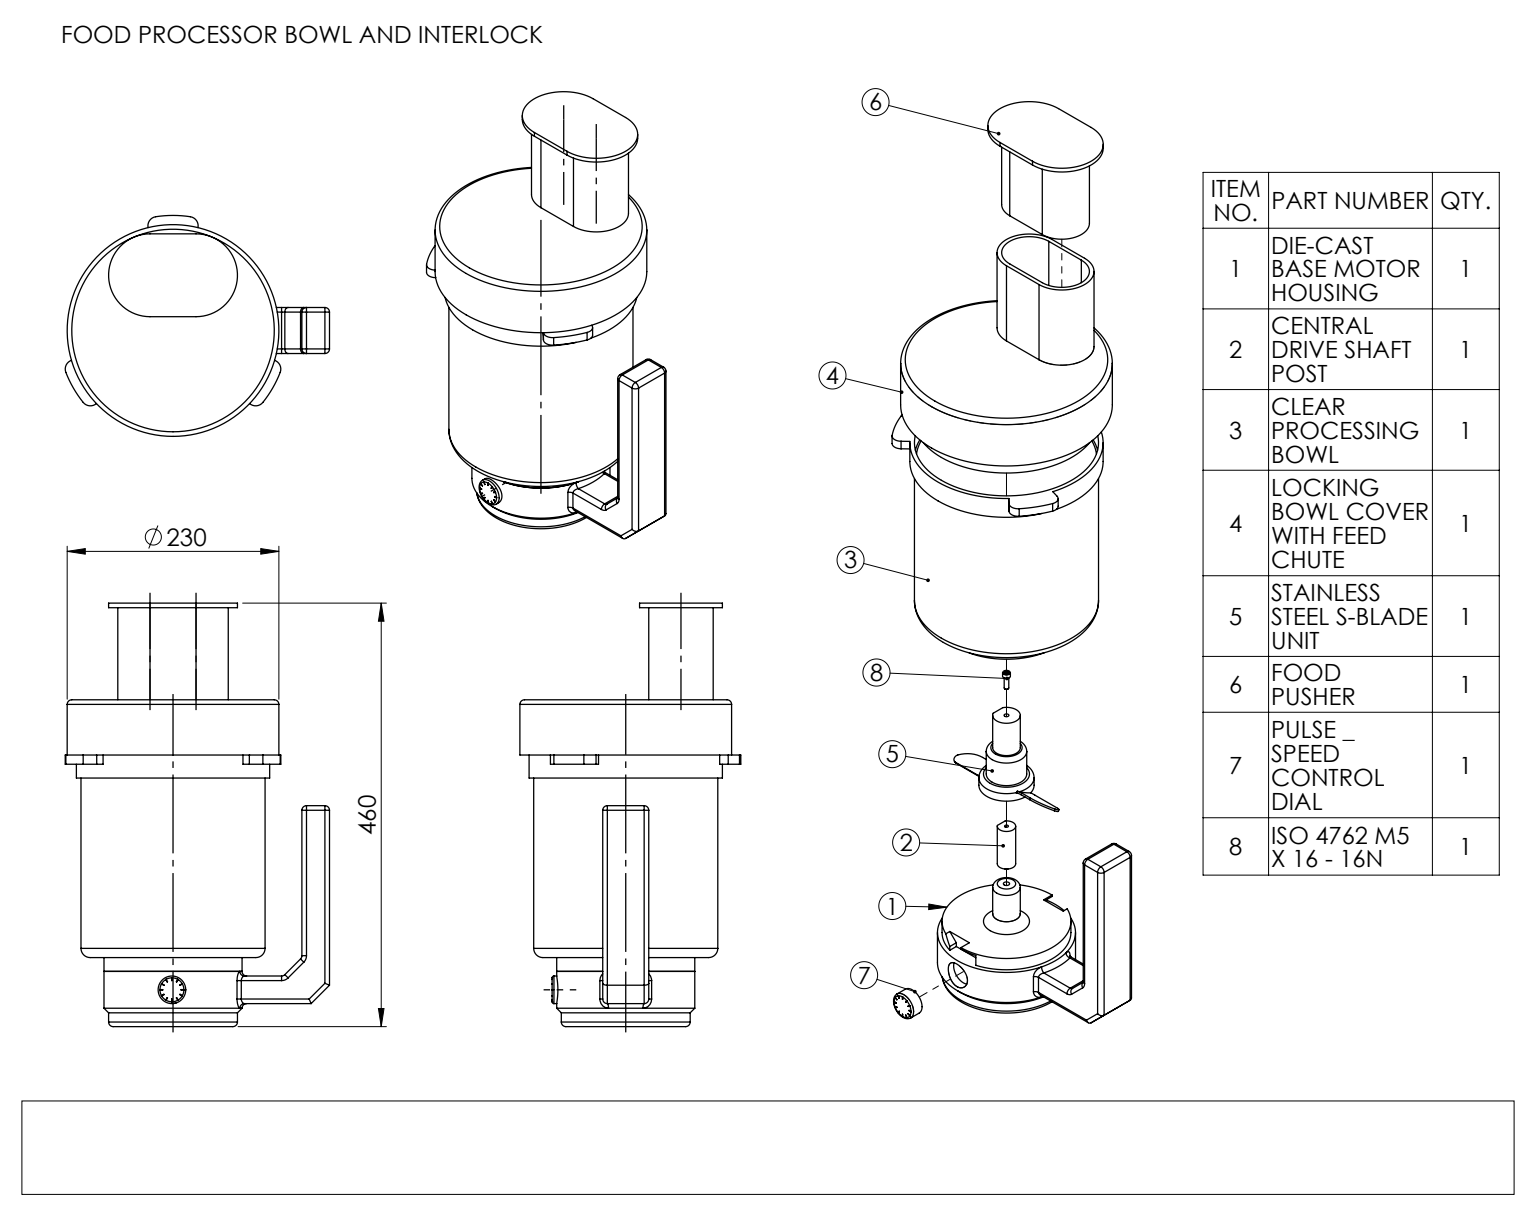
ISO-10303-21;
HEADER;
FILE_DESCRIPTION (('STEP AP214'),
    '1' );
FILE_NAME ('BR-821',
    '2026-10-08T14:59:03',
    ( '' ),
    ( '' ),
    'SwSTEP 2.0',
    'SolidWorks 2026',
    '' );
FILE_SCHEMA (( 'AUTOMOTIVE_DESIGN' ));
ENDSEC;

DATA;
#1 = ORIENTED_EDGE ( 'NONE', *, *, #9406, .F. ) ;
#2 = CARTESIAN_POINT ( 'NONE',  ( 11.80921887069467324, 30.25000000000018474, 79.50000000000000000 ) ) ;
#3 = CARTESIAN_POINT ( 'NONE',  ( 71.93323519045090109, 49.64954395535312415, 21.22984507177767100 ) ) ;
#4 = ORIENTED_EDGE ( 'NONE', *, *, #10707, .F. ) ;
#5 = LINE ( 'NONE', #4817, #10432 ) ;
#6 = PLANE ( 'NONE',  #104 ) ;
#7 = AXIS2_PLACEMENT_3D ( 'NONE', #9543, #8426, #7563 ) ;
#8 = VERTEX_POINT ( 'NONE', #10428 ) ;
#9 = MECHANICAL_DESIGN_GEOMETRIC_PRESENTATION_REPRESENTATION (  '', ( #5399 ), #3796 ) ;
#10 = CARTESIAN_POINT ( 'NONE',  ( 1.836970198721029589E-15, 110.0000000000000000, 15.00000000000000000 ) ) ;
#11 = LINE ( 'NONE', #6448, #10967 ) ;
#12 = CARTESIAN_POINT ( 'NONE',  ( -25.00000000000000000, 445.0000000000000568, -90.00000000000000000 ) ) ;
#13 = CARTESIAN_POINT ( 'NONE',  ( -2.298097038856279806, 112.6250000000000000, -2.298097038856279362 ) ) ;
#14 = CARTESIAN_POINT ( 'NONE',  ( 1.658621287961228320E-16, 111.8124999986344079, 2.708734124999999882 ) ) ;
#15 = ORIENTED_EDGE ( 'NONE', *, *, #10225, .T. ) ;
#16 = AXIS2_PLACEMENT_3D ( 'NONE', #8718, #1999, #3870 ) ;
#17 = ORIENTED_EDGE ( 'NONE', *, *, #3705, .T. ) ;
#18 = CYLINDRICAL_SURFACE ( 'NONE', #1272, 5.000000000000001776 ) ;
#19 = EDGE_CURVE ( 'NONE', #6749, #65, #10302, .T. ) ;
#20 = DIRECTION ( 'NONE',  ( 0.4999999999999933387, -0.8660254037844424824, 0.000000000000000000 ) ) ;
#21 = ORIENTED_EDGE ( 'NONE', *, *, #5442, .F. ) ;
#22 = VECTOR ( 'NONE', #10909, 1000.000000000000000 ) ;
#23 = CARTESIAN_POINT ( 'NONE',  ( -7.907287480251413925, 18.86666975080236597, 80.00000000000000000 ) ) ;
#24 = DIRECTION ( 'NONE',  ( 0.000000000000000000, 0.000000000000000000, -1.000000000000000000 ) ) ;
#25 = CARTESIAN_POINT ( 'NONE',  ( -30.63265341208206038, 76.40790137508867019, 5.685798939282528330 ) ) ;
#26 = CARTESIAN_POINT ( 'NONE',  ( 0.000000000000000000, 153.0000000000000000, 2.099999999999998312 ) ) ;
#27 = EDGE_CURVE ( 'NONE', #1251, #10198, #9485, .T. ) ;
#28 = ORIENTED_EDGE ( 'NONE', *, *, #12033, .F. ) ;
#29 = FACE_OUTER_BOUND ( 'NONE', #6935, .T. ) ;
#30 = UNCERTAINTY_MEASURE_WITH_UNIT (LENGTH_MEASURE( 1.000000000000000082E-05 ), #8409, 'distance_accuracy_value', 'NONE');
#31 = CARTESIAN_POINT ( 'NONE',  ( 74.19588822391826000, 40.66783446091307042, -24.95803700703555350 ) ) ;
#32 = SURFACE_STYLE_FILL_AREA ( #12272 ) ;
#33 = CARTESIAN_POINT ( 'NONE',  ( 0.000000000000000000, 62.00000000000000000, 0.000000000000000000 ) ) ;
#34 = DIRECTION ( 'NONE',  ( 0.000000000000000000, -0.000000000000000000, 1.000000000000000000 ) ) ;
#35 = CARTESIAN_POINT ( 'NONE',  ( 3.250000000000000444, 113.0625000000000000, 1.346194077712559167 ) ) ;
#36 = CARTESIAN_POINT ( 'NONE',  ( 77.29209776116614705, 15.00000000000009059, -20.32449628861697377 ) ) ;
#37 = ORIENTED_EDGE ( 'NONE', *, *, #7691, .T. ) ;
#38 = FACE_BOUND ( 'NONE', #4194, .T. ) ;
#39 = EDGE_CURVE ( 'NONE', #10896, #4898, #9360, .T. ) ;
#40 = CARTESIAN_POINT ( 'NONE',  ( -1.440781129305471087, 43.00000000000008527, 80.00000000000000000 ) ) ;
#41 = VECTOR ( 'NONE', #11324, 1000.000000000000000 ) ;
#42 = ORIENTED_EDGE ( 'NONE', *, *, #4224, .F. ) ;
#43 = CYLINDRICAL_SURFACE ( 'NONE', #5992, 70.00000000000001421 ) ;
#44 = VERTEX_POINT ( 'NONE', #11902 ) ;
#45 = VECTOR ( 'NONE', #2118, 1000.000000000000000 ) ;
#46 = LINE ( 'NONE', #5798, #12120 ) ;
#47 = LINE ( 'NONE', #9767, #6437 ) ;
#48 = EDGE_LOOP ( 'NONE', ( #1031, #6053, #2883, #3031 ) ) ;
#49 = CARTESIAN_POINT ( 'NONE',  ( 30.43737458073258040, 77.00000000000001421, -5.702507482421638407 ) ) ;
#50 = CARTESIAN_POINT ( 'NONE',  ( 170.0000000000011369, 35.00000000000004974, -19.99999999999999645 ) ) ;
#51 = VERTEX_POINT ( 'NONE', #2763 ) ;
#52 = ADVANCED_FACE ( 'NONE', ( #8078 ), #12195, .T. ) ;
#53 = PLANE ( 'NONE',  #708 ) ;
#54 = DIRECTION ( 'NONE',  ( -0.000000000000000000, -1.000000000000000000, -0.000000000000000000 ) ) ;
#55 = DIRECTION ( 'NONE',  ( -0.000000000000000000, -1.000000000000000000, -0.000000000000000000 ) ) ;
#56 = ORIENTED_EDGE ( 'NONE', *, *, #12103, .T. ) ;
#57 = CARTESIAN_POINT ( 'NONE',  ( -1.915364268218909150, 112.6874999986344079, 1.915364268218909594 ) ) ;
#58 = VECTOR ( 'NONE', #5099, 1000.000000000000000 ) ;
#59 = DIRECTION ( 'NONE',  ( 0.000000000000000000, -0.4999999999999976685, 0.8660254037844399289 ) ) ;
#60 = ORIENTED_EDGE ( 'NONE', *, *, #4267, .T. ) ;
#61 = ADVANCED_FACE ( 'NONE', ( #9422 ), #904, .T. ) ;
#62 = CARTESIAN_POINT ( 'NONE',  ( -25.00000000000000000, 345.0000000000000568, -90.00000000000000000 ) ) ;
#63 = ADVANCED_FACE ( 'NONE', ( #7151 ), #4694, .T. ) ;
#64 = CARTESIAN_POINT ( 'NONE',  ( -5.632982942078911925, 15.66369320862007264, 74.78974241430267966 ) ) ;
#65 = VERTEX_POINT ( 'NONE', #3417 ) ;
#66 = CARTESIAN_POINT ( 'NONE',  ( 2.500000000000000000, -1.178949249685214307, 2.042000000000001592 ) ) ;
#67 = ORIENTED_EDGE ( 'NONE', *, *, #12135, .T. ) ;
#68 = AXIS2_PLACEMENT_3D ( 'NONE', #1472, #532, #4327 ) ;
#69 = AXIS2_PLACEMENT_3D ( 'NONE', #2443, #8100, #4365 ) ;
#70 = CARTESIAN_POINT ( 'NONE',  ( -25.00000000000000000, 347.0000000000000568, -88.00000000000000000 ) ) ;
#71 = CARTESIAN_POINT ( 'NONE',  ( 100.7495955565343593, 285.0000000000000568, 29.57226733266770680 ) ) ;
#72 = FACE_BOUND ( 'NONE', #11694, .T. ) ;
#73 = CARTESIAN_POINT ( 'NONE',  ( 5.525725221640833240, 18.86666975080242992, 79.50000000000000000 ) ) ;
#74 = CARTESIAN_POINT ( 'NONE',  ( -3.250000000000000444, 111.5000000000000000, 3.980102097228898231E-16 ) ) ;
#75 = CARTESIAN_POINT ( 'NONE',  ( 72.29554967163173274, 10.06394264408140771, 19.96827991394381030 ) ) ;
#76 = ORIENTED_EDGE ( 'NONE', *, *, #6927, .T. ) ;
#77 = PRESENTATION_STYLE_ASSIGNMENT (( #1089 ) ) ;
#78 = AXIS2_PLACEMENT_3D ( 'NONE', #1523, #2574, #3573 ) ;
#79 = AXIS2_PLACEMENT_3D ( 'NONE', #1491, #4293, #8024 ) ;
#80 = VERTEX_POINT ( 'NONE', #3761 ) ;
#81 = CYLINDRICAL_SURFACE ( 'NONE', #3664, 5.000000000000000888 ) ;
#82 = CYLINDRICAL_SURFACE ( 'NONE', #2511, 15.00000000000000000 ) ;
#83 = EDGE_LOOP ( 'NONE', ( #1644, #11783, #306, #9102 ) ) ;
#84 = DIRECTION ( 'NONE',  ( 0.000000000000000000, 0.000000000000000000, 1.000000000000000000 ) ) ;
#85 = DIRECTION ( 'NONE',  ( -0.000000000000000000, -1.000000000000000000, -0.000000000000000000 ) ) ;
#86 = DIRECTION ( 'NONE',  ( 0.000000000000000000, 1.000000000000000000, 0.000000000000000000 ) ) ;
#87 = CIRCLE ( 'NONE', #695, 73.00000000000002842 ) ;
#88 = AXIS2_PLACEMENT_3D ( 'NONE', #4376, #577, #4254 ) ;
#89 = EDGE_CURVE ( 'NONE', #9269, #3272, #10464, .T. ) ;
#90 = ORIENTED_EDGE ( 'NONE', *, *, #4166, .T. ) ;
#91 = EDGE_CURVE ( 'NONE', #9396, #343, #11975, .T. ) ;
#92 = ADVANCED_FACE ( 'NONE', ( #6517 ), #10949, .F. ) ;
#93 = VECTOR ( 'NONE', #163, 1000.000000000000000 ) ;
#94 = CARTESIAN_POINT ( 'NONE',  ( 74.77359728361332714, 42.68513822356444365, -24.22100760279283094 ) ) ;
#95 = AXIS2_PLACEMENT_3D ( 'NONE', #7431, #12111, #3682 ) ;
#96 = CARTESIAN_POINT ( 'NONE',  ( -1.440781129305282571, 17.00000000000009592, 80.00000000000000000 ) ) ;
#97 = CARTESIAN_POINT ( 'NONE',  ( 25.00000000000000000, 445.0000000000000568, -59.99999999999999289 ) ) ;
#98 = DIRECTION ( 'NONE',  ( 1.000000000000000000, 0.000000000000000000, -3.469446951953613203E-16 ) ) ;
#99 = FACE_OUTER_BOUND ( 'NONE', #3781, .T. ) ;
#100 = ORIENTED_EDGE ( 'NONE', *, *, #2094, .T. ) ;
#101 = CARTESIAN_POINT ( 'NONE',  ( -2.298097038856279362, 111.3750000000000000, 2.298097038856279806 ) ) ;
#102 = PRODUCT ( 'Food Pusher', 'Food Pusher', '', ( #178 ) ) ;
#103 = CARTESIAN_POINT ( 'NONE',  ( 1.121994411437818862, 110.4999999986344079, 2.708734125000000326 ) ) ;
#104 = AXIS2_PLACEMENT_3D ( 'NONE', #11679, #5881, #9664 ) ;
#105 = ORIENTED_EDGE ( 'NONE', *, *, #968, .F. ) ;
#106 = DIRECTION ( 'NONE',  ( -0.000000000000000000, -1.000000000000000000, -0.000000000000000000 ) ) ;
#107 = AXIS2_PLACEMENT_3D ( 'NONE', #11604, #10713, #5802 ) ;
#108 = VERTEX_POINT ( 'NONE', #8368 ) ;
#109 = CARTESIAN_POINT ( 'NONE',  ( 0.000000000000000000, 67.00000000000000000, -73.00000000000002842 ) ) ;
#110 = DIRECTION ( 'NONE',  ( -0.8660254037844363761, 0.5000000000000038858, 0.000000000000000000 ) ) ;
#111 = ORIENTED_EDGE ( 'NONE', *, *, #6676, .F. ) ;
#112 = AXIS2_PLACEMENT_3D ( 'NONE', #12229, #2739, #12169 ) ;
#113 = DIRECTION ( 'NONE',  ( 0.000000000000000000, 1.000000000000000000, 0.000000000000000000 ) ) ;
#114 = CARTESIAN_POINT ( 'NONE',  ( 27.33018067101281900, 86.99999999999998579, 12.37179148263487782 ) ) ;
#115 = ORIENTED_EDGE ( 'NONE', *, *, #11098, .T. ) ;
#116 = CONTEXT_DEPENDENT_SHAPE_REPRESENTATION ( #11241, #9863 ) ;
#117 = DIRECTION ( 'NONE',  ( 1.000000000000000000, -0.000000000000000000, 0.000000000000000000 ) ) ;
#118 = COLOUR_RGB ( '', 0.09019608, 0.27058824, 0.51372549) ;
#119 = LINE ( 'NONE', #1007, #8979 ) ;
#120 = DIRECTION ( 'NONE',  ( -0.2816406412635021894, 0.000000000000000000, 0.9595199576812789566 ) ) ;
#121 = ORIENTED_EDGE ( 'NONE', *, *, #6558, .F. ) ;
#122 = CARTESIAN_POINT ( 'NONE',  ( -1.121994411437818862, 113.6249999986344079, 2.708734125000000326 ) ) ;
#123 = DIRECTION ( 'NONE',  ( 1.000000000000000000, 0.000000000000000000, 0.000000000000000000 ) ) ;
#124 = EDGE_CURVE ( 'NONE', #2418, #8492, #10933, .T. ) ;
#125 = AXIS2_PLACEMENT_3D ( 'NONE', #9417, #9481, #11434 ) ;
#126 = EDGE_LOOP ( 'NONE', ( #8083, #10579, #5308 ) ) ;
#127 = CARTESIAN_POINT ( 'NONE',  ( 89.80805993797383735, 285.0000000000000568, 71.82974571984303225 ) ) ;
#128 = PLANE ( 'NONE',  #8446 ) ;
#129 = ORIENTED_EDGE ( 'NONE', *, *, #8171, .F. ) ;
#130 = CARTESIAN_POINT ( 'NONE',  ( 1.836970198721029589E-15, 115.0000000000000142, 15.00000000000000000 ) ) ;
#131 = DIRECTION ( 'NONE',  ( -1.000000000000000000, -1.387778780781444492E-15, 0.000000000000000000 ) ) ;
#132 = ORIENTED_EDGE ( 'NONE', *, *, #1282, .T. ) ;
#133 = CARTESIAN_POINT ( 'NONE',  ( -1.346194077712560944, 110.3125000000000000, 3.249999999999998668 ) ) ;
#134 = CARTESIAN_POINT ( 'NONE',  ( 69.52686081652184669, 20.00000000000009237, -28.12499999999999645 ) ) ;
#135 = PLANE ( 'NONE',  #4004 ) ;
#136 = CARTESIAN_POINT ( 'NONE',  ( 1.915364268218908705, 114.4374999986344079, -1.915364268218909594 ) ) ;
#137 = CARTESIAN_POINT ( 'NONE',  ( 20.00000000000000000, 7.965803112215716020, -67.08203932499371547 ) ) ;
#138 = CARTESIAN_POINT ( 'NONE',  ( 1.915364268218909150, 112.6874999986344079, 1.915364268218909150 ) ) ;
#139 = ORIENTED_EDGE ( 'NONE', *, *, #323, .F. ) ;
#140 = EDGE_CURVE ( 'NONE', #6671, #381, #10679, .T. ) ;
#141 = ADVANCED_FACE ( 'NONE', ( #5767 ), #10055, .F. ) ;
#142 = EDGE_LOOP ( 'NONE', ( #5615, #3837, #7263, #6163, #8146, #5499, #6846 ) ) ;
#143 = PLANE ( 'NONE',  #4255 ) ;
#144 = DIRECTION ( 'NONE',  ( -0.000000000000000000, -1.000000000000000000, -0.000000000000000000 ) ) ;
#145 = ORIENTED_EDGE ( 'NONE', *, *, #5135, .F. ) ;
#146 = CARTESIAN_POINT ( 'NONE',  ( -75.98513253586241945, 285.0000000000000568, 72.46557550663233371 ) ) ;
#147 = CARTESIAN_POINT ( 'NONE',  ( 75.98513253586142469, 275.0000000000000000, 72.46557550663338532 ) ) ;
#148 = ADVANCED_FACE ( 'NONE', ( #9407 ), #4682, .T. ) ;
#149 = DIRECTION ( 'NONE',  ( -0.000000000000000000, -0.000000000000000000, 1.000000000000000000 ) ) ;
#150 = CARTESIAN_POINT ( 'NONE',  ( -0.9407811293052614765, 20.00000000000009237, 79.50000000000000000 ) ) ;
#151 = ORIENTED_EDGE ( 'NONE', *, *, #4389, .T. ) ;
#152 = AXIS2_PLACEMENT_3D ( 'NONE', #2615, #6425, #9273 ) ;
#153 = EDGE_CURVE ( 'NONE', #12150, #6802, #1695, .T. ) ;
#154 = EDGE_CURVE ( 'NONE', #8296, #4939, #9365, .T. ) ;
#155 = FILL_AREA_STYLE_COLOUR ( '', #11172 ) ;
#156 = ORIENTED_EDGE ( 'NONE', *, *, #11948, .T. ) ;
#157 = CARTESIAN_POINT ( 'NONE',  ( 70.81305327821827689, 40.84876555524851938, -24.93520811514266100 ) ) ;
#158 = AXIS2_PLACEMENT_3D ( 'NONE', #4049, #10649, #3342 ) ;
#159 = CARTESIAN_POINT ( 'NONE',  ( 9.942549119892305498, 36.71650635094628967, 79.50000000000000000 ) ) ;
#160 = MECHANICAL_DESIGN_GEOMETRIC_PRESENTATION_REPRESENTATION (  '', ( #10913 ), #2162 ) ;
#161 = CARTESIAN_POINT ( 'NONE',  ( 0.000000000000000000, 264.9990000000000236, -34.99999999999999289 ) ) ;
#162 = ORIENTED_EDGE ( 'NONE', *, *, #3844, .F. ) ;
#163 = DIRECTION ( 'NONE',  ( -0.000000000000000000, -1.000000000000000000, -0.000000000000000000 ) ) ;
#164 = CARTESIAN_POINT ( 'NONE',  ( 76.56941542346943663, 15.25646994755911656, -21.58911091692574047 ) ) ;
#165 = ORIENTED_EDGE ( 'NONE', *, *, #7969, .F. ) ;
#166 = CARTESIAN_POINT ( 'NONE',  ( 1.224646799147353533E-14, 265.0000000000000000, -100.0000000000000284 ) ) ;
#167 = CARTESIAN_POINT ( 'NONE',  ( 1.658621287961228566E-16, 110.5624999986344079, 2.708734125000000326 ) ) ;
#168 = ORIENTED_EDGE ( 'NONE', *, *, #9268, .F. ) ;
#169 = CARTESIAN_POINT ( 'NONE',  ( -9.976035167149731819, 34.78349364905394481, 80.00000000000000000 ) ) ;
#170 = ORIENTED_EDGE ( 'NONE', *, *, #8169, .T. ) ;
#171 = LINE ( 'NONE', #7782, #5342 ) ;
#172 = DIRECTION ( 'NONE',  ( 1.000000000000000000, 0.000000000000000000, 3.469446951953613203E-16 ) ) ;
#173 = EDGE_LOOP ( 'NONE', ( #129, #2028 ) ) ;
#174 = CARTESIAN_POINT ( 'NONE',  ( 30.14540500433760783, 76.99999999999997158, -4.927060346216586950 ) ) ;
#175 = EDGE_CURVE ( 'NONE', #10718, #2926, #1576, .T. ) ;
#176 = FACE_OUTER_BOUND ( 'NONE', #3457, .T. ) ;
#177 = ORIENTED_EDGE ( 'NONE', *, *, #6032, .T. ) ;
#178 = PRODUCT_CONTEXT ( 'NONE', #12278, 'mechanical' ) ;
#179 = VECTOR ( 'NONE', #1966, 1000.000000000000000 ) ;
#180 = CARTESIAN_POINT ( 'NONE',  ( 11.80921887069467324, 30.00000000000008882, 80.00000000000000000 ) ) ;
#181 = DIRECTION ( 'NONE',  ( 0.000000000000000000, -0.000000000000000000, 1.000000000000000000 ) ) ;
#182 = ORIENTED_EDGE ( 'NONE', *, *, #8491, .F. ) ;
#183 = CARTESIAN_POINT ( 'NONE',  ( -2.708734125000000326, 113.7499999986343937, 1.121994411437818862 ) ) ;
#184 = CARTESIAN_POINT ( 'NONE',  ( -5.970153145843347347E-16, 113.6249999972688158, -3.250000000000000444 ) ) ;
#185 = AXIS2_PLACEMENT_3D ( 'NONE', #6233, #8025, #4294 ) ;
#186 = ORIENTED_EDGE ( 'NONE', *, *, #175, .F. ) ;
#187 = DIRECTION ( 'NONE',  ( -1.000000000000000000, 0.000000000000000000, -0.000000000000000000 ) ) ;
#188 = LINE ( 'NONE', #3126, #12048 ) ;
#189 = ORIENTED_EDGE ( 'NONE', *, *, #4744, .F. ) ;
#190 = DIRECTION ( 'NONE',  ( 0.000000000000000000, 1.000000000000000000, 0.000000000000000000 ) ) ;
#191 = DIRECTION ( 'NONE',  ( -0.5000000000000095479, -0.8660254037844331565, 0.000000000000000000 ) ) ;
#192 = ORIENTED_EDGE ( 'NONE', *, *, #11363, .T. ) ;
#193 = LINE ( 'NONE', #8731, #4891 ) ;
#194 = CARTESIAN_POINT ( 'NONE',  ( 150.0000000000010800, 15.00000000000008882, 20.00000000000000000 ) ) ;
#195 = DIRECTION ( 'NONE',  ( -0.000000000000000000, -0.000000000000000000, 1.000000000000000000 ) ) ;
#196 = EDGE_CURVE ( 'NONE', #8201, #12241, #11240, .T. ) ;
#197 = VECTOR ( 'NONE', #4605, 1000.000000000000000 ) ;
#198 = DIRECTION ( 'NONE',  ( -0.000000000000000000, -1.000000000000000000, 0.000000000000000000 ) ) ;
#199 = CARTESIAN_POINT ( 'NONE',  ( 5.000000000000000888, 0.000000000000000000, 0.000000000000000000 ) ) ;
#200 = EDGE_CURVE ( 'NONE', #12119, #9588, #3746, .T. ) ;
#201 = CARTESIAN_POINT ( 'NONE',  ( 72.61843774138908714, 15.00000000000009059, 18.75000000000000355 ) ) ;
#202 = CIRCLE ( 'NONE', #8371, 5.000000000000000888 ) ;
#203 = ORIENTED_EDGE ( 'NONE', *, *, #11363, .F. ) ;
#204 = VECTOR ( 'NONE', #4922, 1000.000000000000227 ) ;
#205 = ORIENTED_EDGE ( 'NONE', *, *, #4032, .F. ) ;
#206 = VECTOR ( 'NONE', #5383, 1000.000000000000000 ) ;
#207 = PRODUCT ( 'Stainless Steel S-Blade Unit', 'Stainless Steel S-Blade Unit', '', ( #412 ) ) ;
#208 = CARTESIAN_POINT ( 'NONE',  ( 13.11499952929491641, 34.60506461548092716, 73.84520852716261174 ) ) ;
#209 = EDGE_LOOP ( 'NONE', ( #9146, #6174, #8156, #10356 ) ) ;
#210 = DIRECTION ( 'NONE',  ( -0.7071067811865503483, -0.7071067811865447972, -0.000000000000000000 ) ) ;
#211 = DIRECTION ( 'NONE',  ( 0.000000000000000000, 1.000000000000000000, 0.000000000000000000 ) ) ;
#212 = CARTESIAN_POINT ( 'NONE',  ( 0.000000000000000000, 10.00000000000017586, 0.000000000000000000 ) ) ;
#213 = CARTESIAN_POINT ( 'NONE',  ( -7.473072744137204459, 18.61875173514729198, 80.00000000000000000 ) ) ;
#214 = EDGE_CURVE ( 'NONE', #4965, #8588, #3628, .T. ) ;
#215 = EDGE_CURVE ( 'NONE', #8652, #10794, #4622, .T. ) ;
#216 = AXIS2_PLACEMENT_3D ( 'NONE', #7014, #9871, #9743 ) ;
#217 = AXIS2_PLACEMENT_3D ( 'NONE', #5378, #8352, #3567 ) ;
#218 =( LENGTH_UNIT ( ) NAMED_UNIT ( * ) SI_UNIT ( .MILLI., .METRE. ) );
#219 = EDGE_CURVE ( 'NONE', #4313, #6757, #4559, .T. ) ;
#220 = ORIENTED_EDGE ( 'NONE', *, *, #6316, .F. ) ;
#221 = TOROIDAL_SURFACE ( 'NONE', #8577, 17.00000000000000000, 5.000000000000000000 ) ;
#222 = FACE_OUTER_BOUND ( 'NONE', #11804, .T. ) ;
#223 = VECTOR ( 'NONE', #5439, 1000.000000000000000 ) ;
#224 = ADVANCED_FACE ( 'NONE', ( #10291 ), #7552, .F. ) ;
#225 = ADVANCED_FACE ( 'NONE', ( #3686 ), #6591, .F. ) ;
#226 = CARTESIAN_POINT ( 'NONE',  ( 31.26438337082144159, 85.29075299833057500, 9.699751388268191832 ) ) ;
#227 = CARTESIAN_POINT ( 'NONE',  ( 3.245314017740478073E-16, 170.0000000000000000, -2.649999999999993694 ) ) ;
#228 = FACE_OUTER_BOUND ( 'NONE', #12039, .T. ) ;
#229 = CARTESIAN_POINT ( 'NONE',  ( 71.00672680945956472, 11.81742436800341345, -24.14780939829461204 ) ) ;
#230 = EDGE_LOOP ( 'NONE', ( #6810, #2498, #7329, #11688 ) ) ;
#231 = FACE_OUTER_BOUND ( 'NONE', #702, .T. ) ;
#232 = CARTESIAN_POINT ( 'NONE',  ( 2.708734125000000326, 110.3749999986344221, 1.121994411437818862 ) ) ;
#233 = ORIENTED_EDGE ( 'NONE', *, *, #10820, .F. ) ;
#234 = AXIS2_PLACEMENT_3D ( 'NONE', #9468, #5745, #3808 ) ;
#235 = ORIENTED_EDGE ( 'NONE', *, *, #9238, .T. ) ;
#236 = DIRECTION ( 'NONE',  ( 0.000000000000000000, -0.5000000000000013323, -0.8660254037844380415 ) ) ;
#237 = LINE ( 'NONE', #3111, #10805 ) ;
#238 = ORIENTED_EDGE ( 'NONE', *, *, #5725, .T. ) ;
#239 = CARTESIAN_POINT ( 'NONE',  ( -3.250000000000000444, 111.3124999972687874, 1.346194077712559167 ) ) ;
#240 = CARTESIAN_POINT ( 'NONE',  ( -12.32411137850303184, 36.71650635094619730, 80.00000000000000000 ) ) ;
#241 = EDGE_LOOP ( 'NONE', ( #9519, #6626 ) ) ;
#242 = AXIS2_PLACEMENT_3D ( 'NONE', #11636, #6579, #4023 ) ;
#243 = CARTESIAN_POINT ( 'NONE',  ( -7.474274778359198734, 41.38333024919781167, 79.50000000000000000 ) ) ;
#244 = DIRECTION ( 'NONE',  ( 0.000000000000000000, 0.000000000000000000, 1.000000000000000000 ) ) ;
#245 = ORIENTED_EDGE ( 'NONE', *, *, #2310, .T. ) ;
#246 = CARTESIAN_POINT ( 'NONE',  ( -2.708734125000000326, 110.7499999986343937, 1.121994411437818862 ) ) ;
#247 = CYLINDRICAL_SURFACE ( 'NONE', #2591, 40.00000000000000000 ) ;
#248 = EDGE_CURVE ( 'NONE', #3797, #2264, #8566, .T. ) ;
#249 = EDGE_CURVE ( 'NONE', #1174, #5753, #3010, .T. ) ;
#250 = VECTOR ( 'NONE', #7783, 1000.000000000000000 ) ;
#251 = ORIENTED_EDGE ( 'NONE', *, *, #2932, .T. ) ;
#252 = DIRECTION ( 'NONE',  ( -0.000000000000000000, 1.000000000000000000, -0.000000000000000000 ) ) ;
#253 = ADVANCED_FACE ( 'NONE', ( #8231 ), #12053, .T. ) ;
#254 = CYLINDRICAL_SURFACE ( 'NONE', #5879, 5.000000000000000888 ) ;
#255 = ORIENTED_EDGE ( 'NONE', *, *, #4089, .F. ) ;
#256 = CYLINDRICAL_SURFACE ( 'NONE', #8375, 105.0000000000000426 ) ;
#257 = DIRECTION ( 'NONE',  ( -0.000000000000000000, -0.000000000000000000, 1.000000000000000000 ) ) ;
#258 = ORIENTED_EDGE ( 'NONE', *, *, #4138, .F. ) ;
#259 = FACE_OUTER_BOUND ( 'NONE', #8887, .T. ) ;
#260 = LINE ( 'NONE', #1697, #8889 ) ;
#261 = CARTESIAN_POINT ( 'NONE',  ( -20.00000000000000000, 63.00000000000000000, -67.08203932499371547 ) ) ;
#262 = CIRCLE ( 'NONE', #10209, 75.00000000000002842 ) ;
#263 = CARTESIAN_POINT ( 'NONE',  ( -1.915364268218909594, 114.1874999986344079, -1.915364268218908927 ) ) ;
#264 = CARTESIAN_POINT ( 'NONE',  ( -7.474274778359198734, 41.38333024919781167, 80.00000000000000000 ) ) ;
#265 = CARTESIAN_POINT ( 'NONE',  ( -1.915364268218909594, 113.1874999986344079, -1.915364268218908927 ) ) ;
#266 = ORIENTED_EDGE ( 'NONE', *, *, #6038, .T. ) ;
#267 = CIRCLE ( 'NONE', #8819, 105.0000000000000426 ) ;
#268 = ORIENTED_EDGE ( 'NONE', *, *, #4405, .T. ) ;
#269 = PRODUCT_DEFINITION_CONTEXT ( 'detailed design', #4862, 'design' ) ;
#270 = CARTESIAN_POINT ( 'NONE',  ( 167.9289321881356614, 35.85786437626911294, 25.00000000000000000 ) ) ;
#271 = FACE_OUTER_BOUND ( 'NONE', #1182, .T. ) ;
#272 = ORIENTED_EDGE ( 'NONE', *, *, #9842, .T. ) ;
#273 = CARTESIAN_POINT ( 'NONE',  ( 0.000000000000000000, 109.0000000000000000, 0.000000000000000000 ) ) ;
#274 = DIRECTION ( 'NONE',  ( 0.000000000000000000, 1.000000000000000000, 0.000000000000000000 ) ) ;
#275 = CARTESIAN_POINT ( 'NONE',  ( -12.57411137850303540, 36.28349364905398033, 80.00000000000000000 ) ) ;
#276 = DIRECTION ( 'NONE',  ( 0.000000000000000000, 1.000000000000000000, 0.000000000000000000 ) ) ;
#277 = EDGE_CURVE ( 'NONE', #893, #11323, #5445, .T. ) ;
#278 = AXIS2_PLACEMENT_3D ( 'NONE', #5146, #9864, #5953 ) ;
#279 = ORIENTED_EDGE ( 'NONE', *, *, #3805, .F. ) ;
#280 = VECTOR ( 'NONE', #1354, 1000.000000000000000 ) ;
#281 = EDGE_LOOP ( 'NONE', ( #4160, #1583, #966, #3668, #2740 ) ) ;
#282 = ADVANCED_FACE ( 'NONE', ( #8294 ), #7374, .T. ) ;
#283 = DIRECTION ( 'NONE',  ( 1.224646799147352714E-16, 0.000000000000000000, -1.000000000000000000 ) ) ;
#284 = DIRECTION ( 'NONE',  ( -1.000000000000000000, 0.000000000000000000, 0.000000000000000000 ) ) ;
#285 = CIRCLE ( 'NONE', #11657, 98.00000000000001421 ) ;
#286 = CYLINDRICAL_SURFACE ( 'NONE', #8857, 5.000000000000000888 ) ;
#287 = CARTESIAN_POINT ( 'NONE',  ( 72.04420248082787737, 10.24880064609159724, -20.85013644286576096 ) ) ;
#288 = CARTESIAN_POINT ( 'NONE',  ( 70.71657310242180472, 12.52464281459662310, -24.98455589012892375 ) ) ;
#289 = CARTESIAN_POINT ( 'NONE',  ( -1.121994411437820416, 110.9999999986343937, -2.708734124999999882 ) ) ;
#290 = ORIENTED_EDGE ( 'NONE', *, *, #11197, .T. ) ;
#291 = CARTESIAN_POINT ( 'NONE',  ( 1.990051048614449116E-16, 113.1249999972688158, 3.250000000000000444 ) ) ;
#292 =( GEOMETRIC_REPRESENTATION_CONTEXT ( 3 ) GLOBAL_UNCERTAINTY_ASSIGNED_CONTEXT ( ( #10000 ) ) GLOBAL_UNIT_ASSIGNED_CONTEXT ( ( #7020, #9690, #6089 ) ) REPRESENTATION_CONTEXT ( 'NONE', 'WORKASPACE' ) );
#293 = ADVANCED_FACE ( 'NONE', ( #5930 ), #247, .T. ) ;
#294 = CIRCLE ( 'NONE', #3880, 5.000000000000000888 ) ;
#295 = ADVANCED_FACE ( 'NONE', ( #10535 ), #3875, .F. ) ;
#296 = ORIENTED_EDGE ( 'NONE', *, *, #2512, .T. ) ;
#297 = CARTESIAN_POINT ( 'NONE',  ( -7.474274778359196070, 18.61666975080236597, 79.50000000000000000 ) ) ;
#298 = VERTEX_POINT ( 'NONE', #8597 ) ;
#299 = CARTESIAN_POINT ( 'NONE',  ( 0.000000000000000000, 75.00000000000001421, 0.000000000000000000 ) ) ;
#300 = DIRECTION ( 'NONE',  ( 0.000000000000000000, 1.000000000000000000, 0.000000000000000000 ) ) ;
#301 = VERTEX_POINT ( 'NONE', #9472 ) ;
#302 = VECTOR ( 'NONE', #2224, 1000.000000000000000 ) ;
#303 = DIRECTION ( 'NONE',  ( 0.000000000000000000, -0.000000000000000000, 1.000000000000000000 ) ) ;
#304 = EDGE_CURVE ( 'NONE', #3140, #9041, #7672, .T. ) ;
#305 = CARTESIAN_POINT ( 'NONE',  ( 20.00000000000000355, 50.00000000000000000, -57.08203932499370836 ) ) ;
#306 = ORIENTED_EDGE ( 'NONE', *, *, #8983, .F. ) ;
#307 = CLOSED_SHELL ( 'NONE', ( #11275, #6512, #7917, #11356, #3953, #6283, #1808, #1279, #6245, #3383, #11433, #6682, #11026, #12101, #4967, #2002, #12145, #10844, #5599, #3792, #148, #6574, #11472, #11341, #11642, #320 ) ) ;
#308 = CARTESIAN_POINT ( 'NONE',  ( -4.975863863883684959E-16, 111.0624999986344079, -2.708734125000000326 ) ) ;
#309 = AXIS2_PLACEMENT_3D ( 'NONE', #7223, #9134, #8895 ) ;
#310 = CARTESIAN_POINT ( 'NONE',  ( -2.298097038856279362, 114.2499999972688158, 2.298097038856279806 ) ) ;
#311 = AXIS2_PLACEMENT_3D ( 'NONE', #7560, #9353, #11370 ) ;
#312 = ORIENTED_EDGE ( 'NONE', *, *, #4136, .T. ) ;
#313 = CARTESIAN_POINT ( 'NONE',  ( 8.809218870694669690, 30.25000000000019540, 79.50000000000000000 ) ) ;
#314 = CARTESIAN_POINT ( 'NONE',  ( 0.000000000000000000, 63.00000000000000000, 0.000000000000000000 ) ) ;
#315 = ORIENTED_EDGE ( 'NONE', *, *, #5726, .F. ) ;
#316 = CARTESIAN_POINT ( 'NONE',  ( 9.940467135547327970, 23.28469568327612649, 80.00000000000000000 ) ) ;
#317 = PLANE ( 'NONE',  #6694 ) ;
#318 = ORIENTED_EDGE ( 'NONE', *, *, #11318, .F. ) ;
#319 = CARTESIAN_POINT ( 'NONE',  ( 25.00000000000000000, 445.0000000000000568, -59.99999999999999289 ) ) ;
#320 = ADVANCED_FACE ( 'NONE', ( #4060 ), #2414, .F. ) ;
#321 = FACE_OUTER_BOUND ( 'NONE', #2192, .T. ) ;
#322 = CARTESIAN_POINT ( 'NONE',  ( -30.00000000000004263, 65.00000000000000000, 57.08203932499370836 ) ) ;
#323 = EDGE_CURVE ( 'NONE', #2842, #3092, #6377, .T. ) ;
#324 = ORIENTED_EDGE ( 'NONE', *, *, #11720, .F. ) ;
#325 = CARTESIAN_POINT ( 'NONE',  ( -8.000000000000000000, 115.0000000000000000, 5.999999999999998224 ) ) ;
#326 = CARTESIAN_POINT ( 'NONE',  ( 72.18749622575050751, 14.85620204188371041, 20.39421446794931114 ) ) ;
#327 = AXIS2_PLACEMENT_3D ( 'NONE', #339, #3397, #9993 ) ;
#328 = ORIENTED_EDGE ( 'NONE', *, *, #7404, .T. ) ;
#329 = CARTESIAN_POINT ( 'NONE',  ( 72.04250006633340320, 49.74972593579155244, -20.85600298363996430 ) ) ;
#330 = B_SPLINE_CURVE_WITH_KNOTS ( 'NONE', 3,
 ( #6794, #1186, #6609, #4798, #1865, #11603, #5861, #4988, #8525, #7602, #9644, #2863, #10471, #8586, #49, #3865, #174, #7662 ),
 .UNSPECIFIED., .F., .F.,
 ( 4, 2, 2, 2, 2, 2, 2, 2, 4 ),
 ( 2.823925224926892107E-17, 0.0008221565609605404907, 0.001644313121921052792, 0.002466469682881565310, 0.003288626243842077395, 0.004110782804802590347, 0.004932939365763108937, 0.005755095926723627527, 0.006577252487684147851 ),
 .UNSPECIFIED. ) ;
#331 = ORIENTED_EDGE ( 'NONE', *, *, #3823, .F. ) ;
#332 = LINE ( 'NONE', #5020, #6258 ) ;
#333 = CARTESIAN_POINT ( 'NONE',  ( 71.69683552452212894, 49.37956359449864863, 22.01474836615508579 ) ) ;
#334 = VERTEX_POINT ( 'NONE', #4888 ) ;
#335 = CARTESIAN_POINT ( 'NONE',  ( 165.0000000000011369, 37.07106781186552524, -25.00000000000000000 ) ) ;
#336 = CARTESIAN_POINT ( 'NONE',  ( 11.80921887069467324, 30.25000000000018474, 79.50000000000000000 ) ) ;
#337 = VECTOR ( 'NONE', #4948, 1000.000000000000227 ) ;
#338 = EDGE_CURVE ( 'NONE', #9423, #8980, #11374, .T. ) ;
#339 = CARTESIAN_POINT ( 'NONE',  ( 3.061616997868383043E-15, 75.00000000000000000, -25.00000000000000000 ) ) ;
#340 = CARTESIAN_POINT ( 'NONE',  ( 1.121994411437819084, 110.4999999986343937, 2.708734125000000326 ) ) ;
#341 = ORIENTED_EDGE ( 'NONE', *, *, #9592, .T. ) ;
#342 = FILL_AREA_STYLE ('',( #7079 ) ) ;
#343 = VERTEX_POINT ( 'NONE', #2827 ) ;
#344 = DIRECTION ( 'NONE',  ( 0.000000000000000000, 0.000000000000000000, 1.000000000000000000 ) ) ;
#345 = CARTESIAN_POINT ( 'NONE',  ( 5.200000000000002842, 0.000000000000000000, -2.700000000000000622 ) ) ;
#346 = CARTESIAN_POINT ( 'NONE',  ( 0.000000000000000000, 115.0000000000000000, 0.000000000000000000 ) ) ;
#347 = CARTESIAN_POINT ( 'NONE',  ( -30.00000000000004263, 65.00000000000000000, 63.24555320336758513 ) ) ;
#348 = EDGE_CURVE ( 'NONE', #9835, #9973, #11157, .T. ) ;
#349 = DIRECTION ( 'NONE',  ( 0.8660254037844399289, 0.4999999999999977796, 0.000000000000000000 ) ) ;
#350 = CARTESIAN_POINT ( 'NONE',  ( 2.708734124999999882, 114.2499999986344079, -1.121994411437820638 ) ) ;
#351 = EDGE_CURVE ( 'NONE', #5322, #7972, #10426, .T. ) ;
#352 = ORIENTED_EDGE ( 'NONE', *, *, #1928, .T. ) ;
#353 = DIRECTION ( 'NONE',  ( 1.000000000000000000, -0.000000000000000000, 1.224646799147353207E-16 ) ) ;
#354 = EDGE_CURVE ( 'NONE', #3011, #4721, #2953, .T. ) ;
#355 = VECTOR ( 'NONE', #3125, 1000.000000000000000 ) ;
#356 = STYLED_ITEM ( 'NONE', ( #4270 ), #8978 ) ;
#357 = VERTEX_POINT ( 'NONE', #9483 ) ;
#358 = LINE ( 'NONE', #7956, #6249 ) ;
#359 = ORIENTED_EDGE ( 'NONE', *, *, #2691, .F. ) ;
#360 = CARTESIAN_POINT ( 'NONE',  ( 0.000000000000000000, 165.0000000000000000, 0.000000000000000000 ) ) ;
#361 = CARTESIAN_POINT ( 'NONE',  ( 6.000000000000000888, 62.00000000000000000, 60.00000000000002132 ) ) ;
#362 = ORIENTED_EDGE ( 'NONE', *, *, #8065, .F. ) ;
#363 = CARTESIAN_POINT ( 'NONE',  ( 0.000000000000000000, 165.0000000000000000, 0.000000000000000000 ) ) ;
#364 = DIRECTION ( 'NONE',  ( 0.000000000000000000, 0.000000000000000000, -1.000000000000000000 ) ) ;
#365 = EDGE_CURVE ( 'NONE', #6665, #9990, #8676, .T. ) ;
#366 = VERTEX_POINT ( 'NONE', #3827 ) ;
#367 = LINE ( 'NONE', #11973, #3584 ) ;
#368 = EDGE_CURVE ( 'NONE', #12219, #5612, #10551, .T. ) ;
#369 = ORIENTED_EDGE ( 'NONE', *, *, #7765, .T. ) ;
#370 = CARTESIAN_POINT ( 'NONE',  ( 0.000000000000000000, -10.00000000000000000, 0.000000000000000000 ) ) ;
#371 = DIRECTION ( 'NONE',  ( 1.000000000000000000, 0.000000000000000000, 0.000000000000000000 ) ) ;
#372 = ORIENTED_EDGE ( 'NONE', *, *, #5442, .T. ) ;
#373 = CARTESIAN_POINT ( 'NONE',  ( 0.000000000000000000, 87.00000000000000000, 0.000000000000000000 ) ) ;
#374 = CARTESIAN_POINT ( 'NONE',  ( -20.00000000000000355, 50.00000000000000000, 57.08203932499370836 ) ) ;
#375 = ORIENTED_EDGE ( 'NONE', *, *, #3119, .F. ) ;
#376 = EDGE_CURVE ( 'NONE', #4020, #6378, #3189, .T. ) ;
#377 = ADVANCED_FACE ( 'NONE', ( #6817 ), #11436, .F. ) ;
#378 = DIRECTION ( 'NONE',  ( 0.000000000000000000, 0.000000000000000000, -1.000000000000000000 ) ) ;
#379 = DIRECTION ( 'NONE',  ( -0.8660254037844363761, 0.5000000000000038858, 0.000000000000000000 ) ) ;
#380 = DIRECTION ( 'NONE',  ( 1.000000000000000000, 0.000000000000000000, 0.000000000000000000 ) ) ;
#381 = VERTEX_POINT ( 'NONE', #5888 ) ;
#382 = DIRECTION ( 'NONE',  ( -1.000000000000000000, 0.000000000000000000, -0.000000000000000000 ) ) ;
#383 = CARTESIAN_POINT ( 'NONE',  ( 71.54629459846327677, 15.63701415187600219, 22.64784456521646661 ) ) ;
#384 = VECTOR ( 'NONE', #6845, 1000.000000000000000 ) ;
#385 = AXIS2_PLACEMENT_3D ( 'NONE', #9164, #2752, #5571 ) ;
#386 =( GEOMETRIC_REPRESENTATION_CONTEXT ( 3 ) GLOBAL_UNCERTAINTY_ASSIGNED_CONTEXT ( ( #5659 ) ) GLOBAL_UNIT_ASSIGNED_CONTEXT ( ( #9241, #4519, #9302 ) ) REPRESENTATION_CONTEXT ( 'NONE', 'WORKASPACE' ) );
#387 = EDGE_LOOP ( 'NONE', ( #11646, #165 ) ) ;
#388 = PRODUCT_RELATED_PRODUCT_CATEGORY ( 'part', '', ( #1899 ) ) ;
#389 = CARTESIAN_POINT ( 'NONE',  ( 0.000000000000000000, 0.000000000000000000, 79.50000000000000000 ) ) ;
#390 = CARTESIAN_POINT ( 'NONE',  ( 71.02603146012562263, 42.62559916300720175, -24.29862599233076637 ) ) ;
#391 = ORIENTED_EDGE ( 'NONE', *, *, #7352, .F. ) ;
#392 = CARTESIAN_POINT ( 'NONE',  ( 7.594472908539098732, 25.21650635094628257, 79.50000000000000000 ) ) ;
#393 = CARTESIAN_POINT ( 'NONE',  ( 69.65901248891735520, 42.64626312845745559, 27.79625982057034150 ) ) ;
#394 = ORIENTED_EDGE ( 'NONE', *, *, #6090, .T. ) ;
#395 = CARTESIAN_POINT ( 'NONE',  ( 0.000000000000000000, 290.0000000000000568, 0.000000000000000000 ) ) ;
#396 = CIRCLE ( 'NONE', #7375, 0.5000000000000004441 ) ;
#397 = APPLICATION_CONTEXT ( 'automotive_design' ) ;
#398 = CARTESIAN_POINT ( 'NONE',  ( -3.250000000000000444, 112.3124999972687874, 1.346194077712559167 ) ) ;
#399 = CARTESIAN_POINT ( 'NONE',  ( -14.19078112930533209, 29.75000000000008882, 80.00000000000000000 ) ) ;
#400 = DIRECTION ( 'NONE',  ( -1.000000000000000000, 0.000000000000000000, 2.213536252433181319E-16 ) ) ;
#401 = ORIENTED_EDGE ( 'NONE', *, *, #8827, .T. ) ;
#402 = ORIENTED_EDGE ( 'NONE', *, *, #10964, .T. ) ;
#403 = ORIENTED_EDGE ( 'NONE', *, *, #1223, .T. ) ;
#404 = AXIS2_PLACEMENT_3D ( 'NONE', #7515, #853, #5653 ) ;
#405 = EDGE_CURVE ( 'NONE', #1040, #5376, #600, .T. ) ;
#406 = CARTESIAN_POINT ( 'NONE',  ( 0.000000000000000000, -10.00000000000000000, -65.00000000000001421 ) ) ;
#408 = EDGE_CURVE ( 'NONE', #10035, #8931, #706, .T. ) ;
#407 = CARTESIAN_POINT ( 'NONE',  ( 7.344472908538985045, 35.21650635094629678, 80.00000000000000000 ) ) ;
#409 = DIRECTION ( 'NONE',  ( 0.000000000000000000, 0.000000000000000000, -1.000000000000000000 ) ) ;
#410 = AXIS2_PLACEMENT_3D ( 'NONE', #11253, #12309, #8485 ) ;
#411 = CYLINDRICAL_SURFACE ( 'NONE', #9069, 98.00000000000001421 ) ;
#412 = PRODUCT_CONTEXT ( 'NONE', #6769, 'mechanical' ) ;
#413 = TOROIDAL_SURFACE ( 'NONE', #613, 25.00000000000000000, 10.00000000000000000 ) ;
#414 = CARTESIAN_POINT ( 'NONE',  ( -25.00000000000000000, 445.0000000000000568, -24.99999999999998934 ) ) ;
#415 = PRODUCT_DEFINITION_SHAPE ( 'NONE', 'NONE',  #12358 ) ;
#416 = CARTESIAN_POINT ( 'NONE',  ( -2.708734125000000326, 113.8124999986344079, 3.317242575922457132E-16 ) ) ;
#417 = ORIENTED_EDGE ( 'NONE', *, *, #6620, .F. ) ;
#418 = FACE_OUTER_BOUND ( 'NONE', #10833, .T. ) ;
#419 = AXIS2_PLACEMENT_3D ( 'NONE', #2678, #9277, #9505 ) ;
#420 = TOROIDAL_SURFACE ( 'NONE', #1423, 17.00000000000000000, 5.000000000000000000 ) ;
#421 = VERTEX_POINT ( 'NONE', #5825 ) ;
#422 = CARTESIAN_POINT ( 'NONE',  ( 27.33018067101282966, 87.00000000000000000, 12.37179148263486539 ) ) ;
#423 = ORIENTED_EDGE ( 'NONE', *, *, #513, .F. ) ;
#424 = DIRECTION ( 'NONE',  ( 0.000000000000000000, 1.000000000000000000, 0.000000000000000000 ) ) ;
#425 = CARTESIAN_POINT ( 'NONE',  ( 1.285879139104720633E-15, 216.0365690573663926, 10.49999999999999822 ) ) ;
#426 = EDGE_LOOP ( 'NONE', ( #189, #2218, #6237, #8413 ) ) ;
#427 = CIRCLE ( 'NONE', #3428, 30.00000000000000000 ) ;
#428 = CARTESIAN_POINT ( 'NONE',  ( -5.974274778359230709, 38.78525403784446723, 79.50000000000000000 ) ) ;
#429 = AXIS2_PLACEMENT_3D ( 'NONE', #2506, #6308, #1510 ) ;
#430 = CARTESIAN_POINT ( 'NONE',  ( -30.34950626935404827, 87.16600977219412982, -8.947791397837656646 ) ) ;
#431 = ORIENTED_EDGE ( 'NONE', *, *, #7084, .F. ) ;
#432 = DIRECTION ( 'NONE',  ( 0.000000000000000000, 0.000000000000000000, 1.000000000000000000 ) ) ;
#433 = EDGE_CURVE ( 'NONE', #10879, #1577, #8550, .T. ) ;
#434 = VERTEX_POINT ( 'NONE', #4950 ) ;
#435 = EDGE_CURVE ( 'NONE', #12106, #2099, #3183, .T. ) ;
#436 = FACE_OUTER_BOUND ( 'NONE', #4882, .T. ) ;
#437 = CARTESIAN_POINT ( 'NONE',  ( 0.000000000000000000, 65.00000000000000000, 25.00000000000000000 ) ) ;
#438 = ORIENTED_EDGE ( 'NONE', *, *, #2215, .F. ) ;
#439 = DIRECTION ( 'NONE',  ( 0.000000000000000000, 0.000000000000000000, -1.000000000000000000 ) ) ;
#440 = PLANE ( 'NONE',  #3510 ) ;
#441 = EDGE_LOOP ( 'NONE', ( #2108, #9208, #4543, #3626 ) ) ;
#442 = CARTESIAN_POINT ( 'NONE',  ( 2.500000000000000000, 2.357898499370431722, -2.818925648462311528E-15 ) ) ;
#443 = DIRECTION ( 'NONE',  ( 0.000000000000000000, 0.000000000000000000, 1.000000000000000000 ) ) ;
#444 = DIRECTION ( 'NONE',  ( -0.5000000000000051070, 0.000000000000000000, 0.8660254037844355990 ) ) ;
#445 = ORIENTED_EDGE ( 'NONE', *, *, #7746, .T. ) ;
#446 = LINE ( 'NONE', #10918, #2988 ) ;
#447 = CARTESIAN_POINT ( 'NONE',  ( 74.19588822391826000, 19.33216553908705393, 24.95803700703554640 ) ) ;
#448 = EDGE_CURVE ( 'NONE', #1030, #9112, #4774, .T. ) ;
#449 = EDGE_CURVE ( 'NONE', #11346, #9412, #9727, .T. ) ;
#450 = ORIENTED_EDGE ( 'NONE', *, *, #10797, .T. ) ;
#451 = CARTESIAN_POINT ( 'NONE',  ( 74.19409830870891653, 19.27799416224737428, 24.96047248796920570 ) ) ;
#452 = LINE ( 'NONE', #8050, #6872 ) ;
#453 = ORIENTED_EDGE ( 'NONE', *, *, #3293, .T. ) ;
#454 = CARTESIAN_POINT ( 'NONE',  ( 3.250000000000000444, 111.0000000000000000, 0.000000000000000000 ) ) ;
#455 = CARTESIAN_POINT ( 'NONE',  ( 70.92186449036606177, 47.98994378880887979, 24.39573567383822095 ) ) ;
#456 = AXIS2_PLACEMENT_3D ( 'NONE', #1243, #3050, #5051 ) ;
#457 = ORIENTED_EDGE ( 'NONE', *, *, #2614, .F. ) ;
#458 = CARTESIAN_POINT ( 'NONE',  ( -25.00000000000000000, 345.0000000000000568, -29.99999999999999289 ) ) ;
#459 = DIRECTION ( 'NONE',  ( 0.000000000000000000, 0.000000000000000000, 1.000000000000000000 ) ) ;
#460 = FACE_OUTER_BOUND ( 'NONE', #3066, .T. ) ;
#462 = EDGE_LOOP ( 'NONE', ( #8985, #9947, #5228, #8018 ) ) ;
#461 = MANIFOLD_SOLID_BREP ( 'Extrude-Thin3', #9257 ) ;
#463 =( LENGTH_UNIT ( ) NAMED_UNIT ( * ) SI_UNIT ( .MILLI., .METRE. ) );
#464 = ORIENTED_EDGE ( 'NONE', *, *, #4771, .T. ) ;
#465 = AXIS2_PLACEMENT_3D ( 'NONE', #33, #11522, #7021 ) ;
#466 = CARTESIAN_POINT ( 'NONE',  ( 20.00000000000000355, 54.99999999999999289, -57.08203932499370836 ) ) ;
#467 = DIRECTION ( 'NONE',  ( -0.8660254037844398178, -0.4999999999999977796, 0.000000000000000000 ) ) ;
#468 = LINE ( 'NONE', #7942, #9415 ) ;
#469 = LINE ( 'NONE', #10759, #4021 ) ;
#470 = DIRECTION ( 'NONE',  ( -0.000000000000000000, -0.000000000000000000, -1.000000000000000000 ) ) ;
#471 = CARTESIAN_POINT ( 'NONE',  ( 30.49437064397536901, 76.52118294276679933, -5.489589508502957571 ) ) ;
#472 = CARTESIAN_POINT ( 'NONE',  ( 9.516722952433237737, 19.48499374783434845, 74.39444254373731269 ) ) ;
#473 = CIRCLE ( 'NONE', #5663, 90.00000000000002842 ) ;
#474 = CIRCLE ( 'NONE', #4071, 8.000000000000007105 ) ;
#475 = CARTESIAN_POINT ( 'NONE',  ( 25.00000000000000355, 347.0000000000000568, -31.99999999999998579 ) ) ;
#476 = ADVANCED_FACE ( 'NONE', ( #7582 ), #2973, .T. ) ;
#477 = ADVANCED_FACE ( 'NONE', ( #12331 ), #7566, .T. ) ;
#478 = CARTESIAN_POINT ( 'NONE',  ( -4.975863863883684959E-16, 114.0624999986344079, -2.708734125000000326 ) ) ;
#479 = ORIENTED_EDGE ( 'NONE', *, *, #7943, .T. ) ;
#480 = CYLINDRICAL_SURFACE ( 'NONE', #7570, 3.250000000000000444 ) ;
#481 = ADVANCED_FACE ( 'NONE', ( #10318 ), #11460, .T. ) ;
#482 = MANIFOLD_SOLID_BREP ( 'AdvancedHole1', #4496 ) ;
#483 = VECTOR ( 'NONE', #12060, 1000.000000000000000 ) ;
#484 = CIRCLE ( 'NONE', #9229, 5.000000000000004441 ) ;
#485 = ORIENTED_EDGE ( 'NONE', *, *, #3805, .T. ) ;
#486 = LINE ( 'NONE', #3166, #7436 ) ;
#487 = ORIENTED_EDGE ( 'NONE', *, *, #800, .T. ) ;
#488 = DIRECTION ( 'NONE',  ( 0.000000000000000000, 0.000000000000000000, -1.000000000000000000 ) ) ;
#489 = CARTESIAN_POINT ( 'NONE',  ( 2.298097038856279806, 113.9999999972688158, 2.298097038856279806 ) ) ;
#490 = ORIENTED_EDGE ( 'NONE', *, *, #11919, .F. ) ;
#491 = DIRECTION ( 'NONE',  ( 0.000000000000000000, 0.000000000000000000, 1.000000000000000000 ) ) ;
#492 = DIRECTION ( 'NONE',  ( -0.000000000000000000, -1.000000000000000000, -0.000000000000000000 ) ) ;
#493 = AXIS2_PLACEMENT_3D ( 'NONE', #11847, #424, #8951 ) ;
#494 = ORIENTED_EDGE ( 'NONE', *, *, #4807, .F. ) ;
#495 = CARTESIAN_POINT ( 'NONE',  ( 71.93667174376723494, 49.65291573457426466, -21.21818801319906811 ) ) ;
#496 = AXIS2_PLACEMENT_3D ( 'NONE', #3452, #10924, #1457 ) ;
#497 = ORIENTED_EDGE ( 'NONE', *, *, #5720, .F. ) ;
#498 = DIRECTION ( 'NONE',  ( -0.000000000000000000, -1.000000000000000000, -0.000000000000000000 ) ) ;
#499 = CARTESIAN_POINT ( 'NONE',  ( 1.990051048614449116E-16, 114.1249999972688158, 3.250000000000000444 ) ) ;
#500 = VECTOR ( 'NONE', #3071, 1000.000000000000000 ) ;
#501 = EDGE_LOOP ( 'NONE', ( #8334, #7320, #8092, #12051 ) ) ;
#502 = DIRECTION ( 'NONE',  ( 0.000000000000000000, -1.000000000000000000, -0.000000000000000000 ) ) ;
#503 = DIRECTION ( 'NONE',  ( -1.224646799147352961E-16, 0.000000000000000000, 1.000000000000000000 ) ) ;
#504 = ORIENTED_EDGE ( 'NONE', *, *, #8965, .F. ) ;
#505 = DIRECTION ( 'NONE',  ( 0.000000000000000000, 0.000000000000000000, -1.000000000000000000 ) ) ;
#506 = CARTESIAN_POINT ( 'NONE',  ( -29.63582346253862454, 77.00000000000000000, 4.660254037844413944 ) ) ;
#507 = CARTESIAN_POINT ( 'NONE',  ( 9.184850993605151889E-15, 65.00000000000000000, 75.00000000000002842 ) ) ;
#508 = ORIENTED_EDGE ( 'NONE', *, *, #996, .T. ) ;
#509 = CARTESIAN_POINT ( 'NONE',  ( 2.298097038856279806, 112.1250000000000000, 2.298097038856279806 ) ) ;
#510 = EDGE_CURVE ( 'NONE', #4808, #2880, #3913, .T. ) ;
#511 = CARTESIAN_POINT ( 'NONE',  ( 75.64991689405157160, 16.00507543303197266, 23.01117105493013781 ) ) ;
#512 = CIRCLE ( 'NONE', #11671, 4.999999999999996447 ) ;
#513 = EDGE_CURVE ( 'NONE', #872, #9323, #1788, .T. ) ;
#514 = VECTOR ( 'NONE', #9075, 1000.000000000000000 ) ;
#515 = ORIENTED_EDGE ( 'NONE', *, *, #3965, .F. ) ;
#516 = CARTESIAN_POINT ( 'NONE',  ( -107.1104145097476987, 275.0000000000000000, 41.86118851095882576 ) ) ;
#517 = CARTESIAN_POINT ( 'NONE',  ( -5.974274778359230709, 38.78525403784446723, 80.00000000000000000 ) ) ;
#518 = ORIENTED_EDGE ( 'NONE', *, *, #9580, .T. ) ;
#519 = CYLINDRICAL_SURFACE ( 'NONE', #3271, 98.00000000000001421 ) ;
#520 = CARTESIAN_POINT ( 'NONE',  ( 74.42783152987426831, 41.80108460718831509, 24.66728717810439875 ) ) ;
#521 = ORIENTED_EDGE ( 'NONE', *, *, #9498, .F. ) ;
#522 = DIRECTION ( 'NONE',  ( 0.000000000000000000, 0.000000000000000000, 1.000000000000000000 ) ) ;
#523 = CARTESIAN_POINT ( 'NONE',  ( 0.000000000000000000, 62.00000000000000000, 0.000000000000000000 ) ) ;
#524 = DIRECTION ( 'NONE',  ( 0.000000000000000000, 0.000000000000000000, 1.000000000000000000 ) ) ;
#525 = CARTESIAN_POINT ( 'NONE',  ( 2.708734124999999882, 112.2499999986343937, -1.121994411437820416 ) ) ;
#526 = CIRCLE ( 'NONE', #5716, 73.00000000000002842 ) ;
#527 = ADVANCED_FACE ( 'NONE', ( #2781 ), #9380, .T. ) ;
#528 = EDGE_LOOP ( 'NONE', ( #1296, #3982, #5325, #5454 ) ) ;
#529 = ORIENTED_EDGE ( 'NONE', *, *, #10124, .T. ) ;
#530 = UNCERTAINTY_MEASURE_WITH_UNIT (LENGTH_MEASURE( 1.000000000000000082E-05 ), #1165, 'distance_accuracy_value', 'NONE');
#531 = VECTOR ( 'NONE', #4205, 1000.000000000000000 ) ;
#532 = DIRECTION ( 'NONE',  ( 0.000000000000000000, 1.000000000000000000, 0.000000000000000000 ) ) ;
#533 = CARTESIAN_POINT ( 'NONE',  ( 7.594472908538985045, 34.78349364905407270, 79.50000000000000000 ) ) ;
#534 = CARTESIAN_POINT ( 'NONE',  ( 27.30107202361637775, 86.87046582918780757, 12.43589427268144831 ) ) ;
#535 = CARTESIAN_POINT ( 'NONE',  ( 30.15809951803416666, 76.87504465863048608, -4.876683037773544172 ) ) ;
#536 = CARTESIAN_POINT ( 'NONE',  ( 0.000000000000000000, 170.0000000000000000, 0.000000000000000000 ) ) ;
#537 = EDGE_CURVE ( 'NONE', #9081, #5052, #7524, .T. ) ;
#538 = EDGE_CURVE ( 'NONE', #3006, #5730, #8937, .T. ) ;
#539 = CARTESIAN_POINT ( 'NONE',  ( -11.19078112930532498, 30.25000000000005684, 80.00000000000000000 ) ) ;
#540 = CARTESIAN_POINT ( 'NONE',  ( 1.121994411437819528, 114.1249999986344079, -2.708734124999999882 ) ) ;
#541 = CARTESIAN_POINT ( 'NONE',  ( -1.121994411437819084, 110.8749999986343937, 2.708734124999999882 ) ) ;
#542 = LINE ( 'NONE', #4340, #4784 ) ;
#543 = BREP_WITH_VOIDS ( 'NONE', #9857, ( #2440 ) );
#544 = VERTEX_POINT ( 'NONE', #4970 ) ;
#545 = PRODUCT_DEFINITION ( 'UNKNOWN', '', #11724, #3142 ) ;
#546 = LINE ( 'NONE', #9891, #5841 ) ;
#547 = ORIENTED_EDGE ( 'NONE', *, *, #6712, .T. ) ;
#548 = EDGE_CURVE ( 'NONE', #8705, #7192, #9752, .T. ) ;
#549 = LINE ( 'NONE', #7222, #4086 ) ;
#550 = LINE ( 'NONE', #2356, #9259 ) ;
#551 = ORIENTED_EDGE ( 'NONE', *, *, #4637, .F. ) ;
#552 = CARTESIAN_POINT ( 'NONE',  ( 145.0000000000011369, 225.0000000000000853, 20.00000000000000000 ) ) ;
#553 = DIRECTION ( 'NONE',  ( 1.000000000000000000, 0.000000000000000000, 0.000000000000000000 ) ) ;
#554 = ORIENTED_EDGE ( 'NONE', *, *, #8544, .F. ) ;
#555 = CARTESIAN_POINT ( 'NONE',  ( 71.22480170918208842, 48.64519998125825140, -23.50133972577970809 ) ) ;
#556 = CIRCLE ( 'NONE', #11914, 10.49999999999999822 ) ;
#557 = APPLICATION_CONTEXT ( 'automotive_design' ) ;
#558 = ORIENTED_EDGE ( 'NONE', *, *, #2494, .T. ) ;
#559 = EDGE_CURVE ( 'NONE', #12107, #9423, #10128, .T. ) ;
#560 = DIRECTION ( 'NONE',  ( 0.000000000000000000, 1.000000000000000000, 0.000000000000000000 ) ) ;
#561 = CARTESIAN_POINT ( 'NONE',  ( 20.00000000000000355, 50.00000000000000000, -57.08203932499370836 ) ) ;
#562 = ORIENTED_EDGE ( 'NONE', *, *, #11113, .T. ) ;
#563 = ORIENTED_EDGE ( 'NONE', *, *, #4830, .F. ) ;
#564 = DIRECTION ( 'NONE',  ( 0.000000000000000000, 0.000000000000000000, -1.000000000000000000 ) ) ;
#565 = LINE ( 'NONE', #4363, #10663 ) ;
#566 = CIRCLE ( 'NONE', #6543, 5.000000000000000888 ) ;
#567 = ORIENTED_EDGE ( 'NONE', *, *, #9997, .T. ) ;
#568 = FACE_OUTER_BOUND ( 'NONE', #8692, .T. ) ;
#569 = FACE_OUTER_BOUND ( 'NONE', #2899, .T. ) ;
#570 = FACE_OUTER_BOUND ( 'NONE', #48, .T. ) ;
#571 = EDGE_LOOP ( 'NONE', ( #1015, #10303, #11033, #9480, #6919, #2706, #2009 ) ) ;
#572 = DIRECTION ( 'NONE',  ( 0.000000000000000000, 1.000000000000000000, 0.000000000000000000 ) ) ;
#573 = CARTESIAN_POINT ( 'NONE',  ( 76.47547367680522257, 15.31088028275837232, 21.74308734404365850 ) ) ;
#574 = EDGE_LOOP ( 'NONE', ( #9840, #12059, #508, #10243, #1092 ) ) ;
#575 = ADVANCED_FACE ( 'NONE', ( #222 ), #10757, .T. ) ;
#576 = CARTESIAN_POINT ( 'NONE',  ( 74.16198487095665826, 20.00000000000009237, 25.00000000000000000 ) ) ;
#577 = DIRECTION ( 'NONE',  ( 0.000000000000000000, 1.000000000000000000, 0.000000000000000000 ) ) ;
#578 = EDGE_LOOP ( 'NONE', ( #7010, #3876, #2369, #10990, #1797 ) ) ;
#579 = DIRECTION ( 'NONE',  ( -1.000000000000000000, 0.000000000000000000, 0.000000000000000000 ) ) ;
#580 = CARTESIAN_POINT ( 'NONE',  ( 71.45054378765655656, 44.14136113826621255, 22.96278406504651315 ) ) ;
#581 = ORIENTED_EDGE ( 'NONE', *, *, #4046, .F. ) ;
#582 = EDGE_CURVE ( 'NONE', #2560, #3728, #10872, .T. ) ;
#583 = CARTESIAN_POINT ( 'NONE',  ( 18.80690714323171520, 275.0000000000000000, -123.5771024247852807 ) ) ;
#584 = EDGE_CURVE ( 'NONE', #7474, #5986, #5098, .T. ) ;
#585 = FACE_OUTER_BOUND ( 'NONE', #83, .T. ) ;
#586 = CARTESIAN_POINT ( 'NONE',  ( 1.915364268218908927, 113.1874999986344079, -1.915364268218909816 ) ) ;
#587 = TOROIDAL_SURFACE ( 'NONE', #2379, 9.999999999999998224, 5.000000000000000000 ) ;
#588 = AXIS2_PLACEMENT_3D ( 'NONE', #8725, #5694, #11492 ) ;
#590 = VERTEX_POINT ( 'NONE', #1349 ) ;
#589 = MANIFOLD_SOLID_BREP ( 'Thread1', #307 ) ;
#591 = ORIENTED_EDGE ( 'NONE', *, *, #140, .T. ) ;
#592 = VERTEX_POINT ( 'NONE', #406 ) ;
#593 = DIRECTION ( 'NONE',  ( 0.000000000000000000, 1.000000000000000000, 0.000000000000000000 ) ) ;
#594 = LINE ( 'NONE', #10370, #1166 ) ;
#595 = MECHANICAL_DESIGN_GEOMETRIC_PRESENTATION_REPRESENTATION (  '', ( #5976 ), #2778 ) ;
#596 = EDGE_CURVE ( 'NONE', #11323, #590, #4560, .T. ) ;
#597 = EDGE_CURVE ( 'NONE', #9722, #10814, #8003, .T. ) ;
#598 = DIRECTION ( 'NONE',  ( 1.000000000000000000, 0.000000000000000000, 6.938893903907229610E-17 ) ) ;
#599 = DIRECTION ( 'NONE',  ( 0.000000000000000000, 0.000000000000000000, 1.000000000000000000 ) ) ;
#600 = CIRCLE ( 'NONE', #5380, 9.999999999999994671 ) ;
#601 = CARTESIAN_POINT ( 'NONE',  ( -27.65415084186107109, 87.92311536631548563, -11.47631757750353643 ) ) ;
#602 = LINE ( 'NONE', #5341, #1517 ) ;
#603 = FACE_OUTER_BOUND ( 'NONE', #4240, .T. ) ;
#604 = CARTESIAN_POINT ( 'NONE',  ( 70.00771527461459698, 15.03038860802777776, -26.90815449096327328 ) ) ;
#605 = CARTESIAN_POINT ( 'NONE',  ( 1.346194077712559389, 113.1875000000000142, 3.250000000000000444 ) ) ;
#606 = AXIS2_PLACEMENT_3D ( 'NONE', #1785, #8264, #12267 ) ;
#607 = DIRECTION ( 'NONE',  ( 1.000000000000000000, 0.000000000000000000, 0.000000000000000000 ) ) ;
#608 = EDGE_CURVE ( 'NONE', #8652, #9323, #6330, .T. ) ;
#609 = EDGE_CURVE ( 'NONE', #5087, #6005, #11890, .T. ) ;
#610 = CARTESIAN_POINT ( 'NONE',  ( -1.107447795970746940, 43.00000000000008527, 80.00000000000000000 ) ) ;
#611 = ORIENTED_EDGE ( 'NONE', *, *, #12343, .T. ) ;
#612 = AXIS2_PLACEMENT_3D ( 'NONE', #11738, #4009, #6752 ) ;
#613 = AXIS2_PLACEMENT_3D ( 'NONE', #1971, #10567, #3032 ) ;
#614 = CARTESIAN_POINT ( 'NONE',  ( 27.65415084186298245, 87.92311536631358138, 11.47631757750026438 ) ) ;
#615 = ORIENTED_EDGE ( 'NONE', *, *, #10610, .F. ) ;
#616 = PLANE ( 'NONE',  #7657 ) ;
#617 = DIRECTION ( 'NONE',  ( 0.000000000000000000, 0.000000000000000000, 1.000000000000000000 ) ) ;
#618 = EDGE_LOOP ( 'NONE', ( #8709, #551, #5002, #341 ) ) ;
#619 = CARTESIAN_POINT ( 'NONE',  ( -9.976035167149731819, 34.78349364905394481, 79.50000000000000000 ) ) ;
#620 = CARTESIAN_POINT ( 'NONE',  ( -27.67899820261485999, 88.38261385519929547, -11.05501148229834030 ) ) ;
#621 = ORIENTED_EDGE ( 'NONE', *, *, #3640, .F. ) ;
#622 = DIRECTION ( 'NONE',  ( -0.000000000000000000, 1.000000000000000000, -0.000000000000000000 ) ) ;
#623 = CIRCLE ( 'NONE', #4397, 100.0000000000000284 ) ;
#624 = ORIENTED_EDGE ( 'NONE', *, *, #6789, .F. ) ;
#625 = CIRCLE ( 'NONE', #4207, 5.000000000000000888 ) ;
#626 = CARTESIAN_POINT ( 'NONE',  ( 31.12930703771215235, 75.68563247576862807, -7.901403593909491541 ) ) ;
#627 = CARTESIAN_POINT ( 'NONE',  ( -3.250000000000000444, 114.3749999972688158, 3.980102097228898231E-16 ) ) ;
#628 = ORIENTED_EDGE ( 'NONE', *, *, #8427, .T. ) ;
#629 = DIRECTION ( 'NONE',  ( 0.000000000000000000, 1.000000000000000000, 0.000000000000000000 ) ) ;
#630 = CARTESIAN_POINT ( 'NONE',  ( 69.85388127645428824, 79.49999999999998579, -4.330127018922231841 ) ) ;
#631 = AXIS2_PLACEMENT_3D ( 'NONE', #5538, #3719, #4470 ) ;
#632 = VERTEX_POINT ( 'NONE', #11072 ) ;
#633 = DIRECTION ( 'NONE',  ( -0.000000000000000000, -1.000000000000000000, -0.000000000000000000 ) ) ;
#634 = CARTESIAN_POINT ( 'NONE',  ( 0.000000000000000000, 340.0000000000000000, 0.000000000000000000 ) ) ;
#635 = CYLINDRICAL_SURFACE ( 'NONE', #1812, 30.00000000000000000 ) ;
#636 = ORIENTED_EDGE ( 'NONE', *, *, #12117, .T. ) ;
#637 = CARTESIAN_POINT ( 'NONE',  ( 2.298097038856278918, 111.8750000000000000, -2.298097038856279806 ) ) ;
#638 = EDGE_CURVE ( 'NONE', #7703, #7018, #7140, .T. ) ;
#639 = EDGE_CURVE ( 'NONE', #4325, #2631, #2857, .T. ) ;
#640 = CARTESIAN_POINT ( 'NONE',  ( 27.65180490099799115, 87.90152798314358051, 11.49631016393330540 ) ) ;
#641 = APPLICATION_CONTEXT ( 'automotive_design' ) ;
#642 = AXIS2_PLACEMENT_3D ( 'NONE', #10504, #11452, #9314 ) ;
#643 = EDGE_CURVE ( 'NONE', #2035, #9573, #11004, .T. ) ;
#644 = ORIENTED_EDGE ( 'NONE', *, *, #7376, .F. ) ;
#645 = DIRECTION ( 'NONE',  ( 0.000000000000000000, -0.000000000000000000, 1.000000000000000000 ) ) ;
#646 = CARTESIAN_POINT ( 'NONE',  ( 30.00000000000003908, 65.00000000000000000, -57.08203932499370836 ) ) ;
#647 = ORIENTED_EDGE ( 'NONE', *, *, #8392, .F. ) ;
#648 = FACE_OUTER_BOUND ( 'NONE', #3660, .T. ) ;
#649 = DIRECTION ( 'NONE',  ( 0.000000000000000000, 1.000000000000000000, 0.000000000000000000 ) ) ;
#650 = ORIENTED_EDGE ( 'NONE', *, *, #2819, .T. ) ;
#651 = LINE ( 'NONE', #12127, #2432 ) ;
#652 = DIRECTION ( 'NONE',  ( 8.659560562354884787E-17, 0.7071067811865514585, -0.7071067811865435759 ) ) ;
#653 = CARTESIAN_POINT ( 'NONE',  ( 1.121994411437819528, 114.1249999986344079, -2.708734124999999882 ) ) ;
#654 = CIRCLE ( 'NONE', #3836, 8.000000000000007105 ) ;
#655 = CARTESIAN_POINT ( 'NONE',  ( 1.121994411437818862, 111.7499999986344079, 2.708734124999999882 ) ) ;
#656 = ORIENTED_EDGE ( 'NONE', *, *, #8171, .T. ) ;
#657 = FILL_AREA_STYLE_COLOUR ( '', #970 ) ;
#658 = AXIS2_PLACEMENT_3D ( 'NONE', #9211, #5493, #5618 ) ;
#659 = CARTESIAN_POINT ( 'NONE',  ( 27.02024436599224444, 285.0000000000000568, -111.3324139431193203 ) ) ;
#660 = CARTESIAN_POINT ( 'NONE',  ( 0.000000000000000000, 264.9990000000000236, -59.99999999999999289 ) ) ;
#661 = CARTESIAN_POINT ( 'NONE',  ( -45.35898384862240107, 86.99999999999997158, -8.660254037844424602 ) ) ;
#662 = FACE_BOUND ( 'NONE', #2461, .T. ) ;
#663 = LINE ( 'NONE', #3470, #9246 ) ;
#664 = CARTESIAN_POINT ( 'NONE',  ( 3.678949249685231848, 0.000000000000000000, 0.000000000000000000 ) ) ;
#665 = DIRECTION ( 'NONE',  ( -0.000000000000000000, -1.000000000000000000, -0.000000000000000000 ) ) ;
#666 = CARTESIAN_POINT ( 'NONE',  ( 1.151167991198512444E-14, 67.00000000000000000, -90.00000000000002842 ) ) ;
#667 = EDGE_LOOP ( 'NONE', ( #12006, #10960, #1141, #1963 ) ) ;
#668 = CARTESIAN_POINT ( 'NONE',  ( -5.970153145843347347E-16, 112.7500000000000000, -3.250000000000000444 ) ) ;
#669 = VECTOR ( 'NONE', #12025, 1000.000000000000000 ) ;
#670 = CYLINDRICAL_SURFACE ( 'NONE', #2203, 10.49999999999999822 ) ;
#671 = EDGE_CURVE ( 'NONE', #7769, #10587, #7043, .T. ) ;
#672 = DIRECTION ( 'NONE',  ( 0.000000000000000000, 1.000000000000000000, 0.000000000000000000 ) ) ;
#673 = ORIENTED_EDGE ( 'NONE', *, *, #10831, .F. ) ;
#674 = CYLINDRICAL_SURFACE ( 'NONE', #5648, 15.00000000000000000 ) ;
#675 = AXIS2_PLACEMENT_3D ( 'NONE', #3704, #10435, #7632 ) ;
#676 = CARTESIAN_POINT ( 'NONE',  ( -30.00100000000000122, 77.00000000000000000, -8.660254037844445918 ) ) ;
#677 = DIRECTION ( 'NONE',  ( 1.000000000000000000, 0.000000000000000000, 0.000000000000000000 ) ) ;
#678 = EDGE_LOOP ( 'NONE', ( #186, #9403, #7670, #10826, #1970 ) ) ;
#679 = CARTESIAN_POINT ( 'NONE',  ( 0.000000000000000000, 65.00000000000000000, 0.000000000000000000 ) ) ;
#680 = LINE ( 'NONE', #8276, #8746 ) ;
#681 = EDGE_CURVE ( 'NONE', #7265, #8236, #4523, .T. ) ;
#682 = ORIENTED_EDGE ( 'NONE', *, *, #3384, .F. ) ;
#683 = ADVANCED_FACE ( 'NONE', ( #4455, #3529 ), #8312, .T. ) ;
#684 = CARTESIAN_POINT ( 'NONE',  ( 25.00000000000000000, 445.0000000000000568, -59.99999999999999289 ) ) ;
#685 = AXIS2_PLACEMENT_3D ( 'NONE', #9077, #3726, #10139 ) ;
#686 = VERTEX_POINT ( 'NONE', #466 ) ;
#687 = ORIENTED_EDGE ( 'NONE', *, *, #7241, .F. ) ;
#688 = CARTESIAN_POINT ( 'NONE',  ( 34.77127485704751564, 76.44489695195846934, -8.339765143629700006 ) ) ;
#689 = LINE ( 'NONE', #7424, #4842 ) ;
#690 = ORIENTED_EDGE ( 'NONE', *, *, #7585, .T. ) ;
#691 = DIRECTION ( 'NONE',  ( 0.000000000000000000, -0.8660254037844407060, -0.4999999999999965028 ) ) ;
#692 = PLANE ( 'NONE',  #2879 ) ;
#693 = VERTEX_POINT ( 'NONE', #659 ) ;
#694 = CARTESIAN_POINT ( 'NONE',  ( 0.000000000000000000, 0.000000000000000000, 0.000000000000000000 ) ) ;
#695 = AXIS2_PLACEMENT_3D ( 'NONE', #10958, #11786, #9012 ) ;
#696 = CYLINDRICAL_SURFACE ( 'NONE', #1896, 17.50000000000000000 ) ;
#697 = AXIS2_PLACEMENT_3D ( 'NONE', #6869, #3941, #4122 ) ;
#698 = PLANE ( 'NONE',  #5126 ) ;
#699 = CARTESIAN_POINT ( 'NONE',  ( -24.76446302067273209, 275.0000000000000000, -102.0378428393002679 ) ) ;
#700 = ADVANCED_FACE ( 'NONE', ( #5336 ), #7838, .T. ) ;
#701 = EDGE_CURVE ( 'NONE', #2446, #6472, #11195, .T. ) ;
#702 = EDGE_LOOP ( 'NONE', ( #8992, #2188, #4464, #4778, #1132, #2997, #10050, #6228, #2644, #12301, #5312, #7784, #1821, #3752, #12332, #4684, #6118, #9409, #9392, #3995, #6001 ) ) ;
#703 = DIRECTION ( 'NONE',  ( 1.000000000000000000, 0.000000000000000000, 0.000000000000000000 ) ) ;
#704 = CARTESIAN_POINT ( 'NONE',  ( 0.000000000000000000, 110.0000000000000000, 0.000000000000000000 ) ) ;
#705 = MECHANICAL_DESIGN_GEOMETRIC_PRESENTATION_REPRESENTATION (  '', ( #6077 ), #292 ) ;
#706 = B_SPLINE_CURVE_WITH_KNOTS ( 'NONE', 3,
 ( #3890, #11502, #7747, #11561 ),
 .UNSPECIFIED., .F., .F.,
 ( 4, 4 ),
 ( 0.000000000000000000, 0.001357209897699670955 ),
 .UNSPECIFIED. ) ;
#707 = VECTOR ( 'NONE', #7770, 1000.000000000000000 ) ;
#708 = AXIS2_PLACEMENT_3D ( 'NONE', #3868, #1310, #303 ) ;
#709 = EDGE_LOOP ( 'NONE', ( #12315, #3463 ) ) ;
#710 = DIRECTION ( 'NONE',  ( 0.000000000000000000, 0.000000000000000000, 1.000000000000000000 ) ) ;
#711 = CARTESIAN_POINT ( 'NONE',  ( 70.71067811865476926, 40.00000000000009237, 25.00000000000000000 ) ) ;
#712 = VERTEX_POINT ( 'NONE', #10939 ) ;
#713 = EDGE_CURVE ( 'NONE', #590, #6198, #8187, .T. ) ;
#714 = CARTESIAN_POINT ( 'NONE',  ( 74.16198487095665826, 50.00000000000000000, -30.00000000000000355 ) ) ;
#715 = CARTESIAN_POINT ( 'NONE',  ( 72.54053945716880492, 45.08045300297751368, 19.05169875841045624 ) ) ;
#716 = EDGE_LOOP ( 'NONE', ( #6121, #4199, #2055, #8173 ) ) ;
#717 = ADVANCED_FACE ( 'NONE', ( #8066 ), #12010, .T. ) ;
#718 = FACE_OUTER_BOUND ( 'NONE', #11904, .T. ) ;
#719 = COLOUR_RGB ( '', 0.66274510, 0.83137255, 0.94901961) ;
#720 = CARTESIAN_POINT ( 'NONE',  ( 0.000000000000000000, 75.00000000000001421, 0.000000000000000000 ) ) ;
#721 = DIRECTION ( 'NONE',  ( -0.000000000000000000, -1.000000000000000000, -0.000000000000000000 ) ) ;
#722 = CIRCLE ( 'NONE', #921, 40.00000000000000000 ) ;
#723 = CARTESIAN_POINT ( 'NONE',  ( -2.708734124999999882, 110.9999999986343937, 1.121994411437818862 ) ) ;
#724 = EDGE_LOOP ( 'NONE', ( #7478, #11917, #621, #1398 ) ) ;
#725 = AXIS2_PLACEMENT_3D ( 'NONE', #3282, #2404, #5224 ) ;
#726 = B_SPLINE_CURVE_WITH_KNOTS ( 'NONE', 3,
 ( #5759, #4688, #1765, #8421 ),
 .UNSPECIFIED., .F., .F.,
 ( 4, 4 ),
 ( 0.000000000000000000, 0.002001274951694169153 ),
 .UNSPECIFIED. ) ;
#727 = AXIS2_PLACEMENT_3D ( 'NONE', #9151, #8407, #2620 ) ;
#728 = DIRECTION ( 'NONE',  ( 0.000000000000000000, 0.000000000000000000, -1.000000000000000000 ) ) ;
#729 = ADVANCED_FACE ( 'NONE', ( #6392 ), #9115, .T. ) ;
#730 = CARTESIAN_POINT ( 'NONE',  ( 170.0000000000012221, 35.00000000000009948, -22.92893218813452805 ) ) ;
#731 = DIRECTION ( 'NONE',  ( -1.000000000000000000, 0.000000000000000000, 0.000000000000000000 ) ) ;
#732 = DIRECTION ( 'NONE',  ( 0.000000000000000000, 0.000000000000000000, 1.000000000000000000 ) ) ;
#733 = CIRCLE ( 'NONE', #2527, 17.00000000000000000 ) ;
#734 = CARTESIAN_POINT ( 'NONE',  ( 0.000000000000000000, 127.0000000000000000, 0.000000000000000000 ) ) ;
#735 = CARTESIAN_POINT ( 'NONE',  ( -5.626974384805541796, 44.33833482606972609, 74.79022370185268187 ) ) ;
#736 = CARTESIAN_POINT ( 'NONE',  ( 11.99712217873418574, 22.83768897326552505, 74.03455026502679459 ) ) ;
#737 = VERTEX_POINT ( 'NONE', #6210 ) ;
#738 = CARTESIAN_POINT ( 'NONE',  ( 3.250000000000000444, 113.0000000000000000, 0.000000000000000000 ) ) ;
#739 = PLANE ( 'NONE',  #9145 ) ;
#740 = AXIS2_PLACEMENT_3D ( 'NONE', #9032, #11737, #443 ) ;
#741 = CARTESIAN_POINT ( 'NONE',  ( -1.190781129305471087, 43.00000000000008527, 80.00000000000000000 ) ) ;
#742 = EDGE_LOOP ( 'NONE', ( #9342, #3526, #10485, #11102, #11036 ) ) ;
#743 = FACE_BOUND ( 'NONE', #5622, .T. ) ;
#744 = CARTESIAN_POINT ( 'NONE',  ( 0.000000000000000000, 75.00000000000001421, 0.000000000000000000 ) ) ;
#745 = CARTESIAN_POINT ( 'NONE',  ( 0.000000000000000000, 275.0000000000000000, 0.000000000000000000 ) ) ;
#746 = ORIENTED_EDGE ( 'NONE', *, *, #1750, .F. ) ;
#747 = ADVANCED_FACE ( 'NONE', ( #10001, #3466 ), #7268, .F. ) ;
#748 = DIRECTION ( 'NONE',  ( 0.000000000000000000, 0.000000000000000000, 1.000000000000000000 ) ) ;
#749 = EDGE_CURVE ( 'NONE', #980, #10107, #8125, .T. ) ;
#750 = DIRECTION ( 'NONE',  ( -0.000000000000000000, -0.000000000000000000, 1.000000000000000000 ) ) ;
#751 = ORIENTED_EDGE ( 'NONE', *, *, #7330, .F. ) ;
#752 = DIRECTION ( 'NONE',  ( 0.000000000000000000, 0.000000000000000000, 1.000000000000000000 ) ) ;
#753 = ORIENTED_EDGE ( 'NONE', *, *, #537, .T. ) ;
#754 = DIRECTION ( 'NONE',  ( 0.000000000000000000, 1.000000000000000000, 0.000000000000000000 ) ) ;
#756 = ORIENTED_EDGE ( 'NONE', *, *, #4698, .F. ) ;
#755 = FACE_OUTER_BOUND ( 'NONE', #1895, .T. ) ;
#757 = ORIENTED_EDGE ( 'NONE', *, *, #11505, .F. ) ;
#758 = CARTESIAN_POINT ( 'NONE',  ( -25.00000000000000000, 345.0000000000000568, -90.00000000000000000 ) ) ;
#759 = CARTESIAN_POINT ( 'NONE',  ( -34.72842983617974966, 77.03714026276665550, 8.681696978550554888 ) ) ;
#760 = ORIENTED_EDGE ( 'NONE', *, *, #3268, .T. ) ;
#761 = EDGE_CURVE ( 'NONE', #10706, #2323, #7254, .T. ) ;
#762 =( NAMED_UNIT ( * ) SI_UNIT ( $, .STERADIAN. ) SOLID_ANGLE_UNIT ( ) );
#763 = MANIFOLD_SOLID_BREP ( 'M5 Clearance Hole1', #5696 ) ;
#764 = CARTESIAN_POINT ( 'NONE',  ( -1.440781129305471087, 43.00000000000008527, 80.00000000000000000 ) ) ;
#765 = DIRECTION ( 'NONE',  ( 0.000000000000000000, 0.000000000000000000, -1.000000000000000000 ) ) ;
#766 = LINE ( 'NONE', #6554, #1224 ) ;
#767 = AXIS2_PLACEMENT_3D ( 'NONE', #8094, #2433, #6238 ) ;
#768 = EDGE_LOOP ( 'NONE', ( #10087, #10275, #11943, #656 ) ) ;
#769 = CARTESIAN_POINT ( 'NONE',  ( 2.708734124999999437, 114.4999999986344079, -1.121994411437820638 ) ) ;
#770 = EDGE_CURVE ( 'NONE', #5668, #544, #8820, .T. ) ;
#771 = CARTESIAN_POINT ( 'NONE',  ( 27.52813290908668264, 87.44182241851449078, 11.93450069589769136 ) ) ;
#772 = ORIENTED_EDGE ( 'NONE', *, *, #7001, .F. ) ;
#773 = AXIS2_PLACEMENT_3D ( 'NONE', #816, #4609, #12225 ) ;
#774 = LINE ( 'NONE', #11179, #7774 ) ;
#775 = EDGE_CURVE ( 'NONE', #8980, #6431, #10558, .T. ) ;
#776 = MECHANICAL_DESIGN_GEOMETRIC_PRESENTATION_REPRESENTATION (  '', ( #5155 ), #10705 ) ;
#777 = DIRECTION ( 'NONE',  ( 0.000000000000000000, 0.000000000000000000, 1.000000000000000000 ) ) ;
#778 = SHAPE_REPRESENTATION ( 'socket head cap screw_iso_ISO 4762 M5 x 16 - 16N', ( #1612 ), #6744 ) ;
#779 = ORIENTED_EDGE ( 'NONE', *, *, #2337, .T. ) ;
#780 = LINE ( 'NONE', #5636, #5073 ) ;
#781 = CARTESIAN_POINT ( 'NONE',  ( -45.35898384862240107, 65.26794919243121740, 24.98076211353317078 ) ) ;
#782 = ORIENTED_EDGE ( 'NONE', *, *, #11976, .F. ) ;
#783 = CARTESIAN_POINT ( 'NONE',  ( -0.9407811293054709756, 43.00000000000008527, 80.00000000000000000 ) ) ;
#784 = DIRECTION ( 'NONE',  ( 0.000000000000000000, 0.000000000000000000, -1.000000000000000000 ) ) ;
#785 = CARTESIAN_POINT ( 'NONE',  ( 1.915364268218908705, 113.4374999986344079, -1.915364268218909594 ) ) ;
#786 = DIRECTION ( 'NONE',  ( 0.6901483381584130328, 0.000000000000000000, -0.7236679289129654968 ) ) ;
#787 = ORIENTED_EDGE ( 'NONE', *, *, #9770, .F. ) ;
#788 = DIRECTION ( 'NONE',  ( -0.7071067811865433539, 0.7071067811865517916, 0.000000000000000000 ) ) ;
#789 = DIRECTION ( 'NONE',  ( -0.7071067811865495711, -0.7071067811865455743, -0.000000000000000000 ) ) ;
#790 = CARTESIAN_POINT ( 'NONE',  ( 69.52686081652184669, 50.00000000000000000, -28.12500000000000000 ) ) ;
#791 = CIRCLE ( 'NONE', #10362, 10.00000000000000178 ) ;
#792 = CARTESIAN_POINT ( 'NONE',  ( 24.99999999999999645, 445.0000000000000568, -95.00000000000000000 ) ) ;
#793 = DIRECTION ( 'NONE',  ( 0.2816406412634883671, -0.000000000000000000, 0.9595199576812829534 ) ) ;
#794 = CARTESIAN_POINT ( 'NONE',  ( 72.61843774138907293, 10.00000000000017586, 18.75000000000000000 ) ) ;
#795 = CARTESIAN_POINT ( 'NONE',  ( -25.00000000000000000, 445.0000000000000568, -90.00000000000000000 ) ) ;
#796 = CARTESIAN_POINT ( 'NONE',  ( 2.298097038856279806, 112.1250000000000000, 2.298097038856279806 ) ) ;
#797 = DIRECTION ( 'NONE',  ( -0.000000000000000000, -1.000000000000000000, -0.000000000000000000 ) ) ;
#798 = ADVANCED_FACE ( 'NONE', ( #9554 ), #9306, .F. ) ;
#799 = AXIS2_PLACEMENT_3D ( 'NONE', #8396, #2668, #933 ) ;
#800 = EDGE_CURVE ( 'NONE', #51, #8715, #2709, .T. ) ;
#801 = DIRECTION ( 'NONE',  ( 0.000000000000000000, -0.5000000000000013323, -0.8660254037844380415 ) ) ;
#802 = ORIENTED_EDGE ( 'NONE', *, *, #6455, .F. ) ;
#803 = LINE ( 'NONE', #5605, #6040 ) ;
#804 = LINE ( 'NONE', #2726, #2890 ) ;
#805 = CARTESIAN_POINT ( 'NONE',  ( 74.16198487095664404, 20.00000000000008882, -24.99999999999999645 ) ) ;
#806 = EDGE_LOOP ( 'NONE', ( #3816, #1259, #9132, #4908 ) ) ;
#807 = CIRCLE ( 'NONE', #9945, 5.000000000000000888 ) ;
#808 =( REPRESENTATION_RELATIONSHIP ('NONE','NONE', #3713, #11842 ) REPRESENTATION_RELATIONSHIP_WITH_TRANSFORMATION ( #7090 )SHAPE_REPRESENTATION_RELATIONSHIP( ) );
#809 = CARTESIAN_POINT ( 'NONE',  ( 0.000000000000000000, 265.0000000000000000, 0.000000000000000000 ) ) ;
#810 = PLANE ( 'NONE',  #2982 ) ;
#811 = EDGE_LOOP ( 'NONE', ( #487, #3572, #7539, #8514, #12336, #11658, #7127 ) ) ;
#812 = DIRECTION ( 'NONE',  ( -1.000000000000000000, -0.000000000000000000, -0.000000000000000000 ) ) ;
#813 = AXIS2_PLACEMENT_3D ( 'NONE', #4855, #106, #2049 ) ;
#814 = AXIS2_PLACEMENT_3D ( 'NONE', #8418, #12242, #891 ) ;
#815 = ORIENTED_EDGE ( 'NONE', *, *, #3454, .T. ) ;
#816 = CARTESIAN_POINT ( 'NONE',  ( 0.000000000000000000, 122.5000000000000000, 0.000000000000000000 ) ) ;
#818 = ORIENTED_EDGE ( 'NONE', *, *, #6558, .T. ) ;
#817 = DIRECTION ( 'NONE',  ( 0.000000000000000000, 0.000000000000000000, 1.000000000000000000 ) ) ;
#819 = ORIENTED_EDGE ( 'NONE', *, *, #9007, .T. ) ;
#820 = CARTESIAN_POINT ( 'NONE',  ( -31.06657576416735012, 76.26187158480907158, 8.234095398640720376 ) ) ;
#821 = ORIENTED_EDGE ( 'NONE', *, *, #12135, .F. ) ;
#822 = FILL_AREA_STYLE_COLOUR ( '', #4749 ) ;
#823 = LINE ( 'NONE', #3562, #4087 ) ;
#825 = CARTESIAN_POINT ( 'NONE',  ( 2.500000000000000000, 0.000000000000000000, 0.000000000000000000 ) ) ;
#824 = CIRCLE ( 'NONE', #8564, 5.000000000000000888 ) ;
#826 = AXIS2_PLACEMENT_3D ( 'NONE', #4284, #9299, #12253 ) ;
#827 = CARTESIAN_POINT ( 'NONE',  ( 145.0000000000011369, 225.0000000000000853, 20.00000000000000000 ) ) ;
#828 = VERTEX_POINT ( 'NONE', #2897 ) ;
#829 = CARTESIAN_POINT ( 'NONE',  ( 2.708734124999999882, 114.5624999986344079, 0.000000000000000000 ) ) ;
#830 = CARTESIAN_POINT ( 'NONE',  ( 0.000000000000000000, 75.00000000000001421, 0.000000000000000000 ) ) ;
#831 = AXIS2_PLACEMENT_3D ( 'NONE', #8668, #7805, #6747 ) ;
#832 = EDGE_CURVE ( 'NONE', #6075, #1902, #4700, .T. ) ;
#833 = AXIS2_PLACEMENT_3D ( 'NONE', #2685, #5686, #10344 ) ;
#834 = VERTEX_POINT ( 'NONE', #5771 ) ;
#835 = DIRECTION ( 'NONE',  ( -0.000000000000000000, -0.000000000000000000, 1.000000000000000000 ) ) ;
#836 = ORIENTED_EDGE ( 'NONE', *, *, #7826, .F. ) ;
#837 = DIRECTION ( 'NONE',  ( 0.000000000000000000, -0.000000000000000000, 1.000000000000000000 ) ) ;
#838 = CARTESIAN_POINT ( 'NONE',  ( 0.000000000000000000, 63.00000000000000000, 0.000000000000000000 ) ) ;
#839 = ORIENTED_EDGE ( 'NONE', *, *, #3131, .F. ) ;
#840 = DIRECTION ( 'NONE',  ( -0.000000000000000000, -0.000000000000000000, 1.000000000000000000 ) ) ;
#841 = FACE_OUTER_BOUND ( 'NONE', #9772, .T. ) ;
#842 = VECTOR ( 'NONE', #3095, 1000.000000000000000 ) ;
#843 = CARTESIAN_POINT ( 'NONE',  ( -4.975863863883684959E-16, 113.3124999986344079, -2.708734124999999882 ) ) ;
#844 = EDGE_CURVE ( 'NONE', #867, #7067, #11236, .T. ) ;
#845 = CARTESIAN_POINT ( 'NONE',  ( 0.000000000000000000, 65.00000000000000000, 0.000000000000000000 ) ) ;
#846 = ADVANCED_FACE ( 'NONE', ( #8558 ), #18, .T. ) ;
#847 = ORIENTED_EDGE ( 'NONE', *, *, #11408, .T. ) ;
#848 = CARTESIAN_POINT ( 'NONE',  ( -7.474274778359196070, 18.61666975080236597, 79.50000000000000000 ) ) ;
#849 = DIRECTION ( 'NONE',  ( -0.000000000000000000, 1.000000000000000000, -0.000000000000000000 ) ) ;
#850 = AXIS2_PLACEMENT_3D ( 'NONE', #3146, #7011, #2387 ) ;
#851 = ORIENTED_EDGE ( 'NONE', *, *, #11796, .T. ) ;
#852 = CARTESIAN_POINT ( 'NONE',  ( -31.33267436902169933, 77.00000000000000000, 7.087639215986555108 ) ) ;
#853 = DIRECTION ( 'NONE',  ( 0.000000000000000000, 1.000000000000000000, 0.000000000000000000 ) ) ;
#854 = EDGE_CURVE ( 'NONE', #5882, #9199, #10221, .T. ) ;
#855 = DIRECTION ( 'NONE',  ( 0.5000000000000066613, 0.8660254037844347108, 0.000000000000000000 ) ) ;
#856 = DIRECTION ( 'NONE',  ( 0.000000000000000000, 0.000000000000000000, 1.000000000000000000 ) ) ;
#857 = DIRECTION ( 'NONE',  ( 0.000000000000000000, 0.000000000000000000, -1.000000000000000000 ) ) ;
#858 = CIRCLE ( 'NONE', #2242, 5.000000000000000888 ) ;
#859 = CARTESIAN_POINT ( 'NONE',  ( 2.298097038856278918, 112.7499999972688158, -2.298097038856279806 ) ) ;
#860 = CARTESIAN_POINT ( 'NONE',  ( 0.000000000000000000, 62.00000000000000000, 0.000000000000000000 ) ) ;
#861 = VERTEX_POINT ( 'NONE', #10306 ) ;
#862 = PLANE ( 'NONE',  #11013 ) ;
#863 = ADVANCED_FACE ( 'NONE', ( #8621 ), #81, .F. ) ;
#864 = CARTESIAN_POINT ( 'NONE',  ( 0.000000000000000000, 127.0000000000000000, 0.000000000000000000 ) ) ;
#865 = EDGE_CURVE ( 'NONE', #1902, #8652, #11263, .T. ) ;
#866 = CARTESIAN_POINT ( 'NONE',  ( -20.00000000000000355, 7.965803112215716020, 57.08203932499370836 ) ) ;
#867 = VERTEX_POINT ( 'NONE', #7454 ) ;
#868 = VECTOR ( 'NONE', #6176, 1000.000000000000000 ) ;
#869 = PRODUCT_DEFINITION ( 'UNKNOWN', '', #3750, #269 ) ;
#870 = CARTESIAN_POINT ( 'NONE',  ( 0.000000000000000000, 77.00000000000000000, 0.000000000000000000 ) ) ;
#871 = CARTESIAN_POINT ( 'NONE',  ( 8.809218870694669690, 30.25000000000019540, 80.00000000000000000 ) ) ;
#872 = VERTEX_POINT ( 'NONE', #1775 ) ;
#873 = CARTESIAN_POINT ( 'NONE',  ( -5.974274778359230709, 38.78525403784446723, 79.50000000000000000 ) ) ;
#874 = CIRCLE ( 'NONE', #11828, 75.00000000000002842 ) ;
#875 = VERTEX_POINT ( 'NONE', #5586 ) ;
#876 = LINE ( 'NONE', #2799, #9503 ) ;
#877 = DIRECTION ( 'NONE',  ( -3.469446951953613203E-16, 0.000000000000000000, 1.000000000000000000 ) ) ;
#878 = ORIENTED_EDGE ( 'NONE', *, *, #1877, .T. ) ;
#879 = DIRECTION ( 'NONE',  ( 0.4999999999999933387, -0.8660254037844424824, 0.000000000000000000 ) ) ;
#880 = ORIENTED_EDGE ( 'NONE', *, *, #11127, .T. ) ;
#881 = DIRECTION ( 'NONE',  ( 0.000000000000000000, 0.000000000000000000, 1.000000000000000000 ) ) ;
#882 = LINE ( 'NONE', #3739, #11237 ) ;
#883 = LINE ( 'NONE', #4804, #7408 ) ;
#884 = PLANE ( 'NONE',  #9162 ) ;
#885 = VECTOR ( 'NONE', #3261, 1000.000000000000000 ) ;
#886 = ORIENTED_EDGE ( 'NONE', *, *, #12003, .F. ) ;
#887 = CARTESIAN_POINT ( 'NONE',  ( 1.121994411437818862, 112.7499999986343937, 2.708734124999999882 ) ) ;
#888 = AXIS2_PLACEMENT_3D ( 'NONE', #5286, #4097, #5226 ) ;
#889 = CARTESIAN_POINT ( 'NONE',  ( 2.298097038856278918, 113.8750000000000000, -2.298097038856279806 ) ) ;
#890 = ORIENTED_EDGE ( 'NONE', *, *, #376, .T. ) ;
#891 = DIRECTION ( 'NONE',  ( 0.000000000000000000, 0.000000000000000000, 1.000000000000000000 ) ) ;
#892 = CARTESIAN_POINT ( 'NONE',  ( 70.19857488179019356, 45.78302546620885494, 26.40439979598030718 ) ) ;
#893 = VERTEX_POINT ( 'NONE', #5893 ) ;
#894 = AXIS2_PLACEMENT_3D ( 'NONE', #1113, #1048, #3976 ) ;
#895 = CYLINDRICAL_SURFACE ( 'NONE', #7648, 5.000000000000000888 ) ;
#896 = FACE_OUTER_BOUND ( 'NONE', #10777, .T. ) ;
#897 = EDGE_CURVE ( 'NONE', #5507, #7525, #3143, .T. ) ;
#898 = ORIENTED_EDGE ( 'NONE', *, *, #2970, .F. ) ;
#899 = FACE_OUTER_BOUND ( 'NONE', #3260, .T. ) ;
#900 = DIRECTION ( 'NONE',  ( -0.000000000000000000, -0.000000000000000000, 1.000000000000000000 ) ) ;
#901 = EDGE_CURVE ( 'NONE', #7094, #2243, #9622, .T. ) ;
#902 = CARTESIAN_POINT ( 'NONE',  ( 2.708734124999999882, 111.5624999986344079, 0.000000000000000000 ) ) ;
#903 = EDGE_CURVE ( 'NONE', #3768, #6428, #7068, .T. ) ;
#904 = CYLINDRICAL_SURFACE ( 'NONE', #3502, 70.00000000000001421 ) ;
#905 = AXIS2_PLACEMENT_3D ( 'NONE', #2605, #3666, #12028 ) ;
#906 = ORIENTED_EDGE ( 'NONE', *, *, #548, .F. ) ;
#907 = AXIS2_PLACEMENT_3D ( 'NONE', #8234, #11997, #1392 ) ;
#908 = ORIENTED_EDGE ( 'NONE', *, *, #9647, .F. ) ;
#909 = VECTOR ( 'NONE', #8508, 1000.000000000000114 ) ;
#910 = CARTESIAN_POINT ( 'NONE',  ( -25.00000000000000000, 445.0000000000000568, -90.00000000000000000 ) ) ;
#911 = DIRECTION ( 'NONE',  ( 0.000000000000000000, 1.000000000000000000, 0.000000000000000000 ) ) ;
#912 = ORIENTED_EDGE ( 'NONE', *, *, #11212, .F. ) ;
#913 = DIRECTION ( 'NONE',  ( -0.000000000000000000, -1.000000000000000000, -0.000000000000000000 ) ) ;
#914 = VECTOR ( 'NONE', #4848, 1000.000000000000114 ) ;
#915 = LINE ( 'NONE', #11450, #4998 ) ;
#916 = CARTESIAN_POINT ( 'NONE',  ( -7.474274778359196070, 18.61666975080236597, 79.50000000000000000 ) ) ;
#917 = CARTESIAN_POINT ( 'NONE',  ( -5.970153145843347347E-16, 112.7500000000000000, -3.250000000000000444 ) ) ;
#918 = ADVANCED_FACE ( 'NONE', ( #4896 ), #143, .F. ) ;
#919 = ORIENTED_EDGE ( 'NONE', *, *, #10882, .F. ) ;
#920 = DIRECTION ( 'NONE',  ( -0.000000000000000000, -1.000000000000000000, -0.000000000000000000 ) ) ;
#921 = AXIS2_PLACEMENT_3D ( 'NONE', #781, #3754, #11121 ) ;
#922 = UNCERTAINTY_MEASURE_WITH_UNIT (LENGTH_MEASURE( 1.000000000000000082E-05 ), #12072, 'distance_accuracy_value', 'NONE');
#923 = CARTESIAN_POINT ( 'NONE',  ( 72.18749622575050751, 45.14379795811530727, -20.39421446795105197 ) ) ;
#924 = VECTOR ( 'NONE', #4990, 1000.000000000000000 ) ;
#925 = ORIENTED_EDGE ( 'NONE', *, *, #449, .T. ) ;
#926 = EDGE_CURVE ( 'NONE', #6039, #4819, #473, .T. ) ;
#927 = EDGE_CURVE ( 'NONE', #9416, #10602, #9613, .T. ) ;
#928 = CARTESIAN_POINT ( 'NONE',  ( 0.000000000000000000, 170.0000000000000000, 2.649999999999987477 ) ) ;
#929 = DIRECTION ( 'NONE',  ( -0.000000000000000000, -1.000000000000000000, -0.000000000000000000 ) ) ;
#930 = CARTESIAN_POINT ( 'NONE',  ( 69.62792625627730558, 17.67721533924630961, -27.87393767067208827 ) ) ;
#931 = VERTEX_POINT ( 'NONE', #10744 ) ;
#932 = DIRECTION ( 'NONE',  ( 0.000000000000000000, 0.000000000000000000, 1.000000000000000000 ) ) ;
#933 = DIRECTION ( 'NONE',  ( 0.000000000000000000, 0.000000000000000000, 1.000000000000000000 ) ) ;
#934 = VERTEX_POINT ( 'NONE', #7755 ) ;
#935 = DIRECTION ( 'NONE',  ( 0.000000000000000000, 0.000000000000000000, 1.000000000000000000 ) ) ;
#936 = CIRCLE ( 'NONE', #8681, 0.2500000000000002220 ) ;
#937 = EDGE_CURVE ( 'NONE', #2246, #11684, #2206, .T. ) ;
#938 = VERTEX_POINT ( 'NONE', #4137 ) ;
#939 = LINE ( 'NONE', #8710, #3742 ) ;
#940 = LINE ( 'NONE', #12287, #7026 ) ;
#941 = ORIENTED_EDGE ( 'NONE', *, *, #1209, .F. ) ;
#942 = AXIS2_PLACEMENT_3D ( 'NONE', #4143, #10750, #1402 ) ;
#943 = DIRECTION ( 'NONE',  ( 0.000000000000000000, 0.000000000000000000, 1.000000000000000000 ) ) ;
#944 = DIRECTION ( 'NONE',  ( 0.000000000000000000, 0.000000000000000000, 1.000000000000000000 ) ) ;
#945 = VERTEX_POINT ( 'NONE', #2266 ) ;
#946 =( NAMED_UNIT ( * ) SI_UNIT ( $, .STERADIAN. ) SOLID_ANGLE_UNIT ( ) );
#947 = DIRECTION ( 'NONE',  ( 0.000000000000000000, 0.000000000000000000, -1.000000000000000000 ) ) ;
#948 = CYLINDRICAL_SURFACE ( 'NONE', #5812, 25.50000000000000000 ) ;
#949 = CARTESIAN_POINT ( 'NONE',  ( 0.000000000000000000, 122.0000000000000000, 0.000000000000000000 ) ) ;
#950 = VERTEX_POINT ( 'NONE', #2146 ) ;
#951 = CARTESIAN_POINT ( 'NONE',  ( 2.708734124999999882, 112.5624999986344079, 0.000000000000000000 ) ) ;
#952 = CARTESIAN_POINT ( 'NONE',  ( -2.298097038856279362, 111.2499999972688158, 2.298097038856279806 ) ) ;
#953 = EDGE_CURVE ( 'NONE', #9323, #9030, #7991, .T. ) ;
#954 = ORIENTED_EDGE ( 'NONE', *, *, #1330, .T. ) ;
#955 = FACE_OUTER_BOUND ( 'NONE', #3507, .T. ) ;
#956 = EDGE_CURVE ( 'NONE', #3370, #4721, #6850, .T. ) ;
#957 = DIRECTION ( 'NONE',  ( 1.000000000000000000, 0.000000000000000000, 0.000000000000000000 ) ) ;
#958 = ORIENTED_EDGE ( 'NONE', *, *, #6551, .T. ) ;
#959 = DIRECTION ( 'NONE',  ( -0.7071067811865364705, 8.659560562355067211E-17, -0.7071067811865584529 ) ) ;
#960 = DIRECTION ( 'NONE',  ( 0.000000000000000000, 1.000000000000000000, -1.287488025362403787E-15 ) ) ;
#961 = ORIENTED_EDGE ( 'NONE', *, *, #5528, .F. ) ;
#962 = DIRECTION ( 'NONE',  ( 0.000000000000000000, 1.000000000000000000, 0.000000000000000000 ) ) ;
#963 = DIRECTION ( 'NONE',  ( 0.000000000000000000, -1.000000000000000000, 0.000000000000000000 ) ) ;
#964 = CARTESIAN_POINT ( 'NONE',  ( 145.0000000000011369, 67.07106781186550393, -20.00000000000000000 ) ) ;
#965 = CARTESIAN_POINT ( 'NONE',  ( -2.708734124999999882, 114.0624999986344079, 3.317242575922456639E-16 ) ) ;
#966 = ORIENTED_EDGE ( 'NONE', *, *, #9420, .T. ) ;
#967 =( LENGTH_UNIT ( ) NAMED_UNIT ( * ) SI_UNIT ( .MILLI., .METRE. ) );
#968 = EDGE_CURVE ( 'NONE', #9588, #4898, #3082, .T. ) ;
#969 = VECTOR ( 'NONE', #11600, 1000.000000000000114 ) ;
#970 = COLOUR_RGB ( '', 0.72549020, 0.75294118, 0.79215686) ;
#971 = ORIENTED_EDGE ( 'NONE', *, *, #3981, .F. ) ;
#972 = DIRECTION ( 'NONE',  ( 0.000000000000000000, 0.000000000000000000, 1.000000000000000000 ) ) ;
#973 = EDGE_CURVE ( 'NONE', #8579, #2134, #1216, .T. ) ;
#974 = CARTESIAN_POINT ( 'NONE',  ( 2.500000000000000000, 2.357898499370431722, -2.818925648462311528E-15 ) ) ;
#975 = ORIENTED_EDGE ( 'NONE', *, *, #7214, .F. ) ;
#976 = CARTESIAN_POINT ( 'NONE',  ( 2.500000000000000000, 0.000000000000000000, 0.000000000000000000 ) ) ;
#977 = LINE ( 'NONE', #3904, #10328 ) ;
#978 = DIRECTION ( 'NONE',  ( 0.000000000000000000, -1.000000000000000000, 0.000000000000000000 ) ) ;
#979 = PRODUCT_DEFINITION_FORMATION_WITH_SPECIFIED_SOURCE ( 'ANY', '', #10458, .NOT_KNOWN. ) ;
#980 = VERTEX_POINT ( 'NONE', #1154 ) ;
#981 = CARTESIAN_POINT ( 'NONE',  ( 0.000000000000000000, 0.000000000000000000, 0.000000000000000000 ) ) ;
#982 = EDGE_CURVE ( 'NONE', #9665, #9072, #11640, .T. ) ;
#983 = CARTESIAN_POINT ( 'NONE',  ( 71.13813068160534669, 43.14388772265235872, -23.95492789737679828 ) ) ;
#984 = EDGE_LOOP ( 'NONE', ( #5661, #255, #2855, #6607 ) ) ;
#985 = LINE ( 'NONE', #159, #4247 ) ;
#986 = FACE_OUTER_BOUND ( 'NONE', #8799, .T. ) ;
#987 = DIRECTION ( 'NONE',  ( 0.000000000000000000, -0.4999999999999993339, 0.8660254037844390407 ) ) ;
#988 = CARTESIAN_POINT ( 'NONE',  ( 75.64998878962165918, 16.00502810556076838, -23.01105902605769771 ) ) ;
#989 = ORIENTED_EDGE ( 'NONE', *, *, #12075, .T. ) ;
#990 = DIRECTION ( 'NONE',  ( -0.5000000000000012212, 0.000000000000000000, -0.8660254037844379305 ) ) ;
#991 = LINE ( 'NONE', #4979, #7553 ) ;
#992 = AXIS2_PLACEMENT_3D ( 'NONE', #10845, #4177, #11674 ) ;
#993 = ORIENTED_EDGE ( 'NONE', *, *, #10766, .F. ) ;
#994 = MECHANICAL_DESIGN_GEOMETRIC_PRESENTATION_REPRESENTATION (  '', ( #6364 ), #3151 ) ;
#995 = CARTESIAN_POINT ( 'NONE',  ( -3.250000000000000444, 113.3124999972687874, 1.346194077712559167 ) ) ;
#996 = EDGE_CURVE ( 'NONE', #10179, #5363, #332, .T. ) ;
#997 = EDGE_CURVE ( 'NONE', #2035, #8327, #8801, .T. ) ;
#998 = ORIENTED_EDGE ( 'NONE', *, *, #9593, .T. ) ;
#999 = CARTESIAN_POINT ( 'NONE',  ( -25.00000000000000000, 445.0000000000000568, -29.99999999999999289 ) ) ;
#1000 = AXIS2_PLACEMENT_3D ( 'NONE', #873, #12220, #7534 ) ;
#1001 = DIRECTION ( 'NONE',  ( 0.000000000000000000, 0.000000000000000000, 1.000000000000000000 ) ) ;
#1002 = ORIENTED_EDGE ( 'NONE', *, *, #219, .T. ) ;
#1003 = CARTESIAN_POINT ( 'NONE',  ( 73.35315233757310693, 81.28571428571424917, -1.237179148263527928 ) ) ;
#1004 = VERTEX_POINT ( 'NONE', #10865 ) ;
#1005 = APPLICATION_PROTOCOL_DEFINITION ( 'draft international standard', 'automotive_design', 1998, #7643 ) ;
#1006 = FACE_OUTER_BOUND ( 'NONE', #3139, .T. ) ;
#1007 = CARTESIAN_POINT ( 'NONE',  ( 0.000000000000000000, 265.0000000000000000, -98.00000000000001421 ) ) ;
#1008 = PLANE ( 'NONE',  #3807 ) ;
#1009 = ORIENTED_EDGE ( 'NONE', *, *, #2846, .T. ) ;
#1010 = CARTESIAN_POINT ( 'NONE',  ( -2.708734125000000326, 113.1249999986343937, -1.121994411437818195 ) ) ;
#1011 = CARTESIAN_POINT ( 'NONE',  ( -3.250000000000000444, 112.3749999972688158, 3.980102097228898231E-16 ) ) ;
#1012 = ORIENTED_EDGE ( 'NONE', *, *, #175, .T. ) ;
#1013 = CARTESIAN_POINT ( 'NONE',  ( 0.000000000000000000, -5.000000000000000000, 0.000000000000000000 ) ) ;
#1014 = CARTESIAN_POINT ( 'NONE',  ( -12.10445966455964673, 19.69657992720446060, 74.01758460308430188 ) ) ;
#1015 = ORIENTED_EDGE ( 'NONE', *, *, #9080, .T. ) ;
#1016 = DIRECTION ( 'NONE',  ( 0.000000000000000000, -1.000000000000000000, 0.000000000000000000 ) ) ;
#1017 = CARTESIAN_POINT ( 'NONE',  ( 70.07436679451828354, 14.74552910246825199, 26.73229126030999581 ) ) ;
#1018 = AXIS2_PLACEMENT_3D ( 'NONE', #6463, #8626, #10253 ) ;
#1019 = ORIENTED_EDGE ( 'NONE', *, *, #8682, .F. ) ;
#1020 = DIRECTION ( 'NONE',  ( -0.000000000000000000, -1.000000000000000000, -0.000000000000000000 ) ) ;
#1021 = EDGE_CURVE ( 'NONE', #10899, #10965, #7929, .T. ) ;
#1022 = EDGE_CURVE ( 'NONE', #1669, #6843, #3206, .T. ) ;
#1023 = CARTESIAN_POINT ( 'NONE',  ( 0.000000000000000000, 75.00000000000001421, 0.000000000000000000 ) ) ;
#1024 = CARTESIAN_POINT ( 'NONE',  ( -14.19078112930532853, 30.25000000000008882, 80.00000000000000000 ) ) ;
#1025 = DIRECTION ( 'NONE',  ( 0.000000000000000000, 0.000000000000000000, 1.000000000000000000 ) ) ;
#1026 = CARTESIAN_POINT ( 'NONE',  ( -3.250000000000001776, 113.5625000000000000, -1.346194077712558723 ) ) ;
#1027 = AXIS2_PLACEMENT_3D ( 'NONE', #8343, #7711, #5908 ) ;
#1028 = CARTESIAN_POINT ( 'NONE',  ( 77.29025109341935718, 15.00000000000008882, 20.32807234521490614 ) ) ;
#1029 = EDGE_CURVE ( 'NONE', #6450, #6026, #6786, .T. ) ;
#1030 = VERTEX_POINT ( 'NONE', #6887 ) ;
#1031 = ORIENTED_EDGE ( 'NONE', *, *, #1499, .F. ) ;
#1032 = CARTESIAN_POINT ( 'NONE',  ( 13.37359372499693499, 33.71046439641005321, 73.79822922526992102 ) ) ;
#1033 = ORIENTED_EDGE ( 'NONE', *, *, #9798, .T. ) ;
#1034 = CARTESIAN_POINT ( 'NONE',  ( 0.000000000000000000, 265.0000000000000000, 0.000000000000000000 ) ) ;
#1035 = CARTESIAN_POINT ( 'NONE',  ( -20.00000000000000355, 50.00000000000000000, 57.08203932499370836 ) ) ;
#1036 = LINE ( 'NONE', #3773, #6303 ) ;
#1037 = DIRECTION ( 'NONE',  ( 0.000000000000000000, 0.000000000000000000, 1.000000000000000000 ) ) ;
#1038 = EDGE_LOOP ( 'NONE', ( #10956, #1512, #4611, #5247 ) ) ;
#1039 =( LENGTH_UNIT ( ) NAMED_UNIT ( * ) SI_UNIT ( .MILLI., .METRE. ) );
#1040 = VERTEX_POINT ( 'NONE', #4378 ) ;
#1041 = APPLICATION_CONTEXT ( 'automotive_design' ) ;
#1042 = CARTESIAN_POINT ( 'NONE',  ( 69.92278643102426372, 44.50372822854298960, -27.12617897809110801 ) ) ;
#1043 = LINE ( 'NONE', #5844, #11222 ) ;
#1044 = DIRECTION ( 'NONE',  ( 0.000000000000000000, 0.000000000000000000, 1.000000000000000000 ) ) ;
#1045 = CARTESIAN_POINT ( 'NONE',  ( -30.00100000000000122, 87.00000000000000000, 8.660254037844435260 ) ) ;
#1046 = DIRECTION ( 'NONE',  ( 0.4999999999999933387, -0.8660254037844424824, 0.000000000000000000 ) ) ;
#1047 = ORIENTED_EDGE ( 'NONE', *, *, #3864, .F. ) ;
#1048 = DIRECTION ( 'NONE',  ( 0.000000000000000000, 1.000000000000000000, 0.000000000000000000 ) ) ;
#1049 = DIRECTION ( 'NONE',  ( 0.000000000000000000, 0.000000000000000000, 1.000000000000000000 ) ) ;
#1050 = VECTOR ( 'NONE', #3209, 1000.000000000000000 ) ;
#1051 = ADVANCED_FACE ( 'NONE', ( #8112 ), #8052, .T. ) ;
#1052 = EDGE_LOOP ( 'NONE', ( #3247, #9803, #3678, #1729 ) ) ;
#1053 = CARTESIAN_POINT ( 'NONE',  ( -2.298097038856279362, 113.2499999972688158, 2.298097038856279806 ) ) ;
#1054 = ORIENTED_EDGE ( 'NONE', *, *, #10513, .F. ) ;
#1055 = VECTOR ( 'NONE', #1123, 1000.000000000000000 ) ;
#1056 = LINE ( 'NONE', #1122, #1359 ) ;
#1057 = CARTESIAN_POINT ( 'NONE',  ( 75.04216158314673635, 43.19040419545773091, 23.86402193374160774 ) ) ;
#1058 = EDGE_LOOP ( 'NONE', ( #182, #7997, #8845 ) ) ;
#1059 = CARTESIAN_POINT ( 'NONE',  ( 0.000000000000000000, 335.0000000000000000, 0.000000000000000000 ) ) ;
#1060 = ORIENTED_EDGE ( 'NONE', *, *, #9142, .F. ) ;
#1061 = ADVANCED_FACE ( 'NONE', ( #648 ), #5386, .T. ) ;
#1062 = APPLICATION_PROTOCOL_DEFINITION ( 'draft international standard', 'automotive_design', 1998, #6769 ) ;
#1063 = EDGE_CURVE ( 'NONE', #5388, #11288, #3392, .T. ) ;
#1064 = CARTESIAN_POINT ( 'NONE',  ( 2.081899558550500280E-15, 265.0000000000000000, 17.00000000000000000 ) ) ;
#1065 = CYLINDRICAL_SURFACE ( 'NONE', #6806, 44.99999999999999289 ) ;
#1066 = CARTESIAN_POINT ( 'NONE',  ( 0.000000000000000000, 340.0000000000000000, 0.000000000000000000 ) ) ;
#1067 = ORIENTED_EDGE ( 'NONE', *, *, #6888, .T. ) ;
#1068 = CARTESIAN_POINT ( 'NONE',  ( 1.915364268218908927, 113.1874999986344079, -1.915364268218909816 ) ) ;
#1069 = AXIS2_PLACEMENT_3D ( 'NONE', #1304, #9952, #1425 ) ;
#1070 = CARTESIAN_POINT ( 'NONE',  ( -3.250000000000001776, 113.4374999972688300, -1.346194077712558723 ) ) ;
#1071 = EDGE_CURVE ( 'NONE', #4547, #3216, #10105, .T. ) ;
#1072 = ORIENTED_EDGE ( 'NONE', *, *, #1029, .T. ) ;
#1073 = DIRECTION ( 'NONE',  ( -0.000000000000000000, 0.000000000000000000, 1.000000000000000000 ) ) ;
#1074 = FACE_OUTER_BOUND ( 'NONE', #4518, .T. ) ;
#1075 = ORIENTED_EDGE ( 'NONE', *, *, #6041, .F. ) ;
#1076 = CARTESIAN_POINT ( 'NONE',  ( 0.000000000000000000, 165.0000000000000000, 0.000000000000000000 ) ) ;
#1077 = FACE_OUTER_BOUND ( 'NONE', #5495, .T. ) ;
#1078 = ORIENTED_EDGE ( 'NONE', *, *, #956, .T. ) ;
#1079 = EDGE_CURVE ( 'NONE', #10836, #11969, #1581, .T. ) ;
#1080 = EDGE_CURVE ( 'NONE', #366, #8042, #4441, .T. ) ;
#1081 = AXIS2_PLACEMENT_3D ( 'NONE', #8410, #2682, #2741 ) ;
#1082 = PLANE ( 'NONE',  #10248 ) ;
#1083 = CARTESIAN_POINT ( 'NONE',  ( -75.98513253586240523, 275.0000000000000000, 72.46557550663233371 ) ) ;
#1084 = DIRECTION ( 'NONE',  ( -1.000000000000000000, 0.000000000000000000, 0.000000000000000000 ) ) ;
#1085 = DIRECTION ( 'NONE',  ( 0.000000000000000000, -1.000000000000000000, 1.287488025362403787E-15 ) ) ;
#1086 = FACE_OUTER_BOUND ( 'NONE', #6691, .T. ) ;
#1087 = CARTESIAN_POINT ( 'NONE',  ( 77.11525298301567943, 15.03197132203681363, 20.64974928742876159 ) ) ;
#1088 = EDGE_LOOP ( 'NONE', ( #4002, #7356 ) ) ;
#1089 = SURFACE_STYLE_USAGE ( .BOTH. , #2893 ) ;
#1090 = AXIS2_PLACEMENT_3D ( 'NONE', #8302, #9230, #3328 ) ;
#1091 = CIRCLE ( 'NONE', #12038, 2.649999999999993694 ) ;
#1092 = ORIENTED_EDGE ( 'NONE', *, *, #2427, .F. ) ;
#1093 = DIRECTION ( 'NONE',  ( 0.000000000000000000, 0.000000000000000000, 1.000000000000000000 ) ) ;
#1094 = DIRECTION ( 'NONE',  ( -1.000000000000000000, 0.000000000000000000, 0.000000000000000000 ) ) ;
#1095 = VERTEX_POINT ( 'NONE', #1645 ) ;
#1096 = DIRECTION ( 'NONE',  ( -1.000000000000000000, -0.000000000000000000, -0.000000000000000000 ) ) ;
#1097 = LINE ( 'NONE', #4901, #179 ) ;
#1098 = CARTESIAN_POINT ( 'NONE',  ( 9.942549119892305498, 36.71650635094628967, 79.50000000000000000 ) ) ;
#1099 = CARTESIAN_POINT ( 'NONE',  ( -1.915364268218909150, 110.6874999986344079, 1.915364268218909594 ) ) ;
#1100 = CIRCLE ( 'NONE', #7062, 25.00000000000000000 ) ;
#1101 = ORIENTED_EDGE ( 'NONE', *, *, #7916, .T. ) ;
#1102 = AXIS2_PLACEMENT_3D ( 'NONE', #5202, #8863, #11996 ) ;
#1103 = ORIENTED_EDGE ( 'NONE', *, *, #4649, .T. ) ;
#1104 = ORIENTED_EDGE ( 'NONE', *, *, #6468, .T. ) ;
#1105 = ADVANCED_FACE ( 'NONE', ( #11058 ), #8235, .T. ) ;
#1106 = AXIS2_PLACEMENT_3D ( 'NONE', #9506, #3916, #8635 ) ;
#1107 = CARTESIAN_POINT ( 'NONE',  ( 71.43334412524781385, 49.01058866048808227, -22.86096127246359444 ) ) ;
#1108 = CARTESIAN_POINT ( 'NONE',  ( 32.05000697088088657, 85.26794919243110371, 9.660254037844429931 ) ) ;
#1109 = CARTESIAN_POINT ( 'NONE',  ( 0.000000000000000000, 170.0000000000000000, 0.000000000000000000 ) ) ;
#1110 = CARTESIAN_POINT ( 'NONE',  ( -25.00000000000000000, 445.0000000000000568, -29.99999999999999289 ) ) ;
#1111 = CARTESIAN_POINT ( 'NONE',  ( 71.43628325305918736, 10.98492395331197358, -22.85167202658751151 ) ) ;
#1112 = VERTEX_POINT ( 'NONE', #10048 ) ;
#1113 = CARTESIAN_POINT ( 'NONE',  ( 0.000000000000000000, 285.0000000000000568, 0.000000000000000000 ) ) ;
#1114 = PRODUCT_DEFINITION_SHAPE ( 'NONE', 'NONE',  #7780 ) ;
#1115 = CARTESIAN_POINT ( 'NONE',  ( -2.708734125000000326, 110.8124999986344079, 3.317242575922457132E-16 ) ) ;
#1116 = AXIS2_PLACEMENT_3D ( 'NONE', #2438, #7051, #1380 ) ;
#1117 = ORIENTED_EDGE ( 'NONE', *, *, #9037, .T. ) ;
#1118 = LINE ( 'NONE', #9764, #7955 ) ;
#1119 = VECTOR ( 'NONE', #10886, 1000.000000000000000 ) ;
#1120 = ORIENTED_EDGE ( 'NONE', *, *, #11826, .T. ) ;
#1121 = ADVANCED_FACE ( 'NONE', ( #5205 ), #519, .F. ) ;
#1122 = CARTESIAN_POINT ( 'NONE',  ( 2.571758278209433575E-16, 165.0000000000000000, -2.099999999999993427 ) ) ;
#1123 = DIRECTION ( 'NONE',  ( 0.000000000000000000, 1.000000000000000000, 0.000000000000000000 ) ) ;
#1124 = ORIENTED_EDGE ( 'NONE', *, *, #5258, .T. ) ;
#1125 = ADVANCED_FACE ( 'NONE', ( #8177, #12124 ), #9103, .F. ) ;
#1126 = CARTESIAN_POINT ( 'NONE',  ( 0.000000000000000000, 75.00000000000001421, 0.000000000000000000 ) ) ;
#1127 = CARTESIAN_POINT ( 'NONE',  ( 90.45849111412074706, 285.0000000000000568, 86.26854226980164242 ) ) ;
#1128 = ORIENTED_EDGE ( 'NONE', *, *, #4703, .F. ) ;
#1129 = DIRECTION ( 'NONE',  ( 0.000000000000000000, 0.000000000000000000, 1.000000000000000000 ) ) ;
#1130 = CIRCLE ( 'NONE', #1914, 75.00000000000001421 ) ;
#1131 = CARTESIAN_POINT ( 'NONE',  ( 0.000000000000000000, 340.0000000000000000, 0.000000000000000000 ) ) ;
#1132 = ORIENTED_EDGE ( 'NONE', *, *, #7766, .T. ) ;
#1133 = CARTESIAN_POINT ( 'NONE',  ( -1.915364268218909816, 113.9374999986344079, -1.915364268218909150 ) ) ;
#1134 = CARTESIAN_POINT ( 'NONE',  ( -1.346194077712560944, 112.5624999972688158, -3.249999999999999556 ) ) ;
#1135 = VECTOR ( 'NONE', #379, 1000.000000000000114 ) ;
#1136 = ORIENTED_EDGE ( 'NONE', *, *, #4089, .T. ) ;
#1137 = EDGE_CURVE ( 'NONE', #7815, #2386, #7462, .T. ) ;
#1138 = EDGE_CURVE ( 'NONE', #12045, #4325, #2520, .T. ) ;
#1139 = CARTESIAN_POINT ( 'NONE',  ( 7.960204194457798830E-15, -5.000000000000000000, 65.00000000000001421 ) ) ;
#1140 = CARTESIAN_POINT ( 'NONE',  ( -4.134262057974781968, 15.28257175693984848, 74.88765946342873292 ) ) ;
#1141 = ORIENTED_EDGE ( 'NONE', *, *, #11763, .T. ) ;
#1142 = CARTESIAN_POINT ( 'NONE',  ( 0.000000000000000000, 10.00000000000009237, 0.000000000000000000 ) ) ;
#1143 = DIRECTION ( 'NONE',  ( -0.7071067811865364705, 0.000000000000000000, 0.7071067811865584529 ) ) ;
#1144 = ORIENTED_EDGE ( 'NONE', *, *, #10068, .T. ) ;
#1145 = CARTESIAN_POINT ( 'NONE',  ( 0.000000000000000000, 63.00000000000000000, 0.000000000000000000 ) ) ;
#1146 = DIRECTION ( 'NONE',  ( 0.000000000000000000, 0.000000000000000000, 1.000000000000000000 ) ) ;
#1147 = CYLINDRICAL_SURFACE ( 'NONE', #7579, 70.00000000000001421 ) ;
#1148 = DIRECTION ( 'NONE',  ( 0.000000000000000000, 0.000000000000000000, 1.000000000000000000 ) ) ;
#1149 = PLANE ( 'NONE',  #1794 ) ;
#1150 = CARTESIAN_POINT ( 'NONE',  ( 72.53968727264557970, 14.91866686485657922, 19.05499925486891755 ) ) ;
#1151 = ADVANCED_FACE ( 'NONE', ( #7257 ), #11878, .F. ) ;
#1152 = EDGE_CURVE ( 'NONE', #5494, #3256, #5047, .T. ) ;
#1153 = VERTEX_POINT ( 'NONE', #9045 ) ;
#1154 = CARTESIAN_POINT ( 'NONE',  ( 3.061616997868383043E-15, 340.0000000000000000, -84.99999999999998579 ) ) ;
#1155 = DIRECTION ( 'NONE',  ( 0.000000000000000000, 0.000000000000000000, 1.000000000000000000 ) ) ;
#1156 = EDGE_LOOP ( 'NONE', ( #2013, #2025, #6086, #753 ) ) ;
#1157 = DIRECTION ( 'NONE',  ( 0.000000000000000000, 1.000000000000000000, 0.000000000000000000 ) ) ;
#1158 = FACE_OUTER_BOUND ( 'NONE', #10972, .T. ) ;
#1159 = CARTESIAN_POINT ( 'NONE',  ( -31.48070082314331231, 75.91043305631261262, 6.547439342558601716 ) ) ;
#1160 = CARTESIAN_POINT ( 'NONE',  ( 2.708734125000000326, 111.3124999986344079, 0.000000000000000000 ) ) ;
#1161 = ORIENTED_EDGE ( 'NONE', *, *, #3154, .T. ) ;
#1162 = CIRCLE ( 'NONE', #9701, 10.00000000000000178 ) ;
#1163 = CARTESIAN_POINT ( 'NONE',  ( 170.0000000000011369, 30.00000000000008882, 20.00000000000000000 ) ) ;
#1164 = ORIENTED_EDGE ( 'NONE', *, *, #9842, .F. ) ;
#1165 =( LENGTH_UNIT ( ) NAMED_UNIT ( * ) SI_UNIT ( .MILLI., .METRE. ) );
#1166 = VECTOR ( 'NONE', #6523, 1000.000000000000227 ) ;
#1167 = DIRECTION ( 'NONE',  ( 0.000000000000000000, 1.000000000000000000, 0.000000000000000000 ) ) ;
#1168 = CARTESIAN_POINT ( 'NONE',  ( -2.708734125000000326, 112.1249999986343937, -1.121994411437818195 ) ) ;
#1169 =( BOUNDED_CURVE ( )  B_SPLINE_CURVE ( 3, ( #7961, #10837, #3366, #8897 ),
 .UNSPECIFIED., .F., .F. ) 
 B_SPLINE_CURVE_WITH_KNOTS ( ( 4, 4 ),
 ( 1.143370257677567281, 1.145717000886475878 ),
 .UNSPECIFIED. ) 
 CURVE ( )  GEOMETRIC_REPRESENTATION_ITEM ( )  RATIONAL_B_SPLINE_CURVE ( ( 1.000000000000000000, 0.9999995410664119788, 0.9999995410664119788, 1.000000000000000000 ) ) 
 REPRESENTATION_ITEM ( '' )  );
#1170 = CARTESIAN_POINT ( 'NONE',  ( -1.440781129305282571, 17.00000000000009592, 79.50000000000000000 ) ) ;
#1171 = ORIENTED_EDGE ( 'NONE', *, *, #2583, .F. ) ;
#1172 = DIRECTION ( 'NONE',  ( -0.000000000000000000, -1.000000000000000000, -0.000000000000000000 ) ) ;
#1173 = CARTESIAN_POINT ( 'NONE',  ( 75.22303488722339182, 16.54275665089875247, -23.61575757524069630 ) ) ;
#1174 = VERTEX_POINT ( 'NONE', #4317 ) ;
#1175 = CARTESIAN_POINT ( 'NONE',  ( -7.907287480251421030, 41.13333024919781167, 80.00000000000000000 ) ) ;
#1176 = EDGE_CURVE ( 'NONE', #7950, #1521, #6563, .T. ) ;
#1177 = EDGE_CURVE ( 'NONE', #334, #8, #726, .T. ) ;
#1178 = DIRECTION ( 'NONE',  ( -0.000000000000000000, -1.000000000000000000, 0.000000000000000000 ) ) ;
#1179 = ORIENTED_EDGE ( 'NONE', *, *, #11127, .F. ) ;
#1180 = DIRECTION ( 'NONE',  ( 0.000000000000000000, 0.000000000000000000, -1.000000000000000000 ) ) ;
#1181 = ADVANCED_FACE ( 'NONE', ( #10357 ), #10419, .F. ) ;
#1182 = EDGE_LOOP ( 'NONE', ( #9699, #464, #7429, #10894 ) ) ;
#1183 = CARTESIAN_POINT ( 'NONE',  ( -69.85388127645425982, 75.26794919243111792, 7.660254037844449471 ) ) ;
#1184 = CARTESIAN_POINT ( 'NONE',  ( 74.31403689601796714, 41.40717934585230608, 24.81089180822486284 ) ) ;
#1185 = ORIENTED_EDGE ( 'NONE', *, *, #4989, .T. ) ;
#1186 = CARTESIAN_POINT ( 'NONE',  ( 34.45294269781049223, 77.00000000000002842, -8.660253777987195534 ) ) ;
#1187 = PLANE ( 'NONE',  #3304 ) ;
#1188 = ORIENTED_EDGE ( 'NONE', *, *, #2623, .T. ) ;
#1189 = PRODUCT_CONTEXT ( 'NONE', #1041, 'mechanical' ) ;
#1190 = CIRCLE ( 'NONE', #1215, 12.99999999999999822 ) ;
#1191 = CARTESIAN_POINT ( 'NONE',  ( 20.00000000000000000, 50.00000000000000000, -67.08203932499371547 ) ) ;
#1192 = CARTESIAN_POINT ( 'NONE',  ( 0.000000000000000000, 265.0000000000000000, 0.000000000000000000 ) ) ;
#1193 = ORIENTED_EDGE ( 'NONE', *, *, #4561, .T. ) ;
#1194 = CARTESIAN_POINT ( 'NONE',  ( 2.708734125000000326, 111.3124999986344079, 0.000000000000000000 ) ) ;
#1195 = CARTESIAN_POINT ( 'NONE',  ( -3.250000000000000444, 111.3749999972688158, 3.980102097228898231E-16 ) ) ;
#1196 = ORIENTED_EDGE ( 'NONE', *, *, #3655, .T. ) ;
#1197 = DIRECTION ( 'NONE',  ( 0.4999999999999878431, -0.8660254037844455910, 0.000000000000000000 ) ) ;
#1198 = CARTESIAN_POINT ( 'NONE',  ( -5.139633753169690955, 15.51989858384737531, 74.82538224130733795 ) ) ;
#1199 = VERTEX_POINT ( 'NONE', #3692 ) ;
#1200 = DIRECTION ( 'NONE',  ( 0.000000000000000000, 0.000000000000000000, 1.000000000000000000 ) ) ;
#1201 = CARTESIAN_POINT ( 'NONE',  ( 25.00000000000000000, 570.2996408614167194, -59.99999999999999289 ) ) ;
#1202 = ORIENTED_EDGE ( 'NONE', *, *, #12075, .F. ) ;
#1203 = PLANE ( 'NONE',  #10847 ) ;
#1204 = DIRECTION ( 'NONE',  ( -0.8660254037844363761, 0.5000000000000038858, 0.000000000000000000 ) ) ;
#1205 = DIRECTION ( 'NONE',  ( -0.000000000000000000, -1.000000000000000000, 0.000000000000000000 ) ) ;
#1206 = VECTOR ( 'NONE', #6312, 1000.000000000000000 ) ;
#1207 = CARTESIAN_POINT ( 'NONE',  ( -12.57411137850303540, 36.28349364905398033, 79.50000000000000000 ) ) ;
#1208 = CARTESIAN_POINT ( 'NONE',  ( -73.35315233757310693, 79.55366347814538130, 0.2371791482635408899 ) ) ;
#1209 = EDGE_CURVE ( 'NONE', #931, #7101, #5, .T. ) ;
#1210 = CARTESIAN_POINT ( 'NONE',  ( 1.121994411437819084, 112.3749999986344079, -2.708734124999999437 ) ) ;
#1211 = AXIS2_PLACEMENT_3D ( 'NONE', #1906, #1843, #856 ) ;
#1212 = ORIENTED_EDGE ( 'NONE', *, *, #9053, .T. ) ;
#1213 = VECTOR ( 'NONE', #5291, 1000.000000000000000 ) ;
#1214 = ORIENTED_EDGE ( 'NONE', *, *, #1804, .T. ) ;
#1215 = AXIS2_PLACEMENT_3D ( 'NONE', #7760, #3839, #7636 ) ;
#1216 = LINE ( 'NONE', #10621, #3070 ) ;
#1217 = CARTESIAN_POINT ( 'NONE',  ( 4.520246555170921887, 43.87820047625252329, 74.86495189574776532 ) ) ;
#1218 = ORIENTED_EDGE ( 'NONE', *, *, #3200, .F. ) ;
#1219 = DIRECTION ( 'NONE',  ( 0.000000000000000000, 0.000000000000000000, 1.000000000000000000 ) ) ;
#1220 = FACE_OUTER_BOUND ( 'NONE', #8472, .T. ) ;
#1221 = DIRECTION ( 'NONE',  ( 0.000000000000000000, 0.000000000000000000, -1.000000000000000000 ) ) ;
#1222 = EDGE_CURVE ( 'NONE', #10746, #3370, #3820, .T. ) ;
#1223 = EDGE_CURVE ( 'NONE', #9534, #3450, #11896, .T. ) ;
#1224 = VECTOR ( 'NONE', #12235, 1000.000000000000000 ) ;
#1225 = VECTOR ( 'NONE', #7313, 1000.000000000000227 ) ;
#1226 = VECTOR ( 'NONE', #7740, 1000.000000000000000 ) ;
#1227 = DIRECTION ( 'NONE',  ( 0.000000000000000000, 0.000000000000000000, 1.000000000000000000 ) ) ;
#1228 = AXIS2_PLACEMENT_3D ( 'NONE', #11079, #4530, #5225 ) ;
#1229 = CARTESIAN_POINT ( 'NONE',  ( 3.980102097228898231E-16, 110.0000000000000000, -3.250000000000000444 ) ) ;
#1230 = DIRECTION ( 'NONE',  ( -0.000000000000000000, 1.000000000000000000, -0.000000000000000000 ) ) ;
#1231 = VERTEX_POINT ( 'NONE', #3634 ) ;
#1232 = DIRECTION ( 'NONE',  ( 0.000000000000000000, 0.000000000000000000, 1.000000000000000000 ) ) ;
#1233 = CARTESIAN_POINT ( 'NONE',  ( 71.26309188267669015, 11.28349307498528020, -23.38502809576078079 ) ) ;
#1234 = CARTESIAN_POINT ( 'NONE',  ( 70.96538090731310433, 11.90979482576331883, -24.26905913879961929 ) ) ;
#1235 = CARTESIAN_POINT ( 'NONE',  ( 2.708734125000000326, 112.3749999986344221, 1.121994411437818862 ) ) ;
#1236 = VERTEX_POINT ( 'NONE', #1708 ) ;
#1237 = LINE ( 'NONE', #1924, #204 ) ;
#1238 = AXIS2_PLACEMENT_3D ( 'NONE', #1784, #6529, #6582 ) ;
#1239 =( BOUNDED_CURVE ( )  B_SPLINE_CURVE ( 2, ( #499, #8154, #2434, #10086, #627, #11860, #10030, #5367, #11982 ),
 .UNSPECIFIED., .F., .F. ) 
 B_SPLINE_CURVE_WITH_KNOTS ( ( 3, 2, 2, 2, 3 ),
 ( 0.8125000000000006661, 0.8437500000000006661, 0.8750000000000006661, 0.9062500000000007772, 0.9375000000000007772 ),
 .UNSPECIFIED. ) 
 CURVE ( )  GEOMETRIC_REPRESENTATION_ITEM ( )  RATIONAL_B_SPLINE_CURVE ( ( 0.9999999999999983347, 0.9238795325112884038, 1.000000000000000000, 0.9238795325112867385, 1.000000000000000000, 0.9238795325112867385, 1.000000000000000000, 0.9238795325112848511, 1.000000000000001998 ) ) 
 REPRESENTATION_ITEM ( '' )  );
#1240 = EDGE_CURVE ( 'NONE', #1030, #3768, #780, .T. ) ;
#1241 = ORIENTED_EDGE ( 'NONE', *, *, #2131, .F. ) ;
#1242 = ADVANCED_FACE ( 'NONE', ( #12247 ), #895, .T. ) ;
#1243 = CARTESIAN_POINT ( 'NONE',  ( 29.48150359603894088, 275.0000000000000000, -121.4736224277384053 ) ) ;
#1244 = VERTEX_POINT ( 'NONE', #11309 ) ;
#1245 = CARTESIAN_POINT ( 'NONE',  ( 0.000000000000000000, 65.00000000000000000, 0.000000000000000000 ) ) ;
#1246 = CARTESIAN_POINT ( 'NONE',  ( 27.32044479829590244, 86.95653975047672191, 12.39329872843003066 ) ) ;
#1247 = EDGE_LOOP ( 'NONE', ( #4101, #9105, #8582, #1067 ) ) ;
#1248 = AXIS2_PLACEMENT_3D ( 'NONE', #10310, #6332, #2532 ) ;
#1249 = CARTESIAN_POINT ( 'NONE',  ( 2.020667218593133416E-14, 65.00000000000000000, 70.00000000000000000 ) ) ;
#1250 = DIRECTION ( 'NONE',  ( 0.000000000000000000, 1.000000000000000000, 0.000000000000000000 ) ) ;
#1251 = VERTEX_POINT ( 'NONE', #6624 ) ;
#1252 = CARTESIAN_POINT ( 'NONE',  ( 2.708734124999999882, 111.2499999986344079, -1.121994411437820638 ) ) ;
#1253 = CARTESIAN_POINT ( 'NONE',  ( 3.249999999999999556, 113.8124999972688016, -1.346194077712561610 ) ) ;
#1254 = CIRCLE ( 'NONE', #10203, 100.0000000000000142 ) ;
#1255 = ORIENTED_EDGE ( 'NONE', *, *, #4032, .T. ) ;
#1256 = EDGE_CURVE ( 'NONE', #1921, #9884, #2097, .T. ) ;
#1257 = CARTESIAN_POINT ( 'NONE',  ( 29.92433840049366012, 87.25972750007186107, 9.110115264091716014 ) ) ;
#1258 = DIRECTION ( 'NONE',  ( 1.000000000000000000, 0.000000000000000000, 0.000000000000000000 ) ) ;
#1259 = ORIENTED_EDGE ( 'NONE', *, *, #11128, .F. ) ;
#1260 = FACE_OUTER_BOUND ( 'NONE', #11178, .T. ) ;
#1261 = CARTESIAN_POINT ( 'NONE',  ( -24.76446302067273209, 275.0000000000000000, -102.0378428393002679 ) ) ;
#1262 = ORIENTED_EDGE ( 'NONE', *, *, #11781, .T. ) ;
#1263 = CARTESIAN_POINT ( 'NONE',  ( -2.298097038856279362, 110.3750000000000000, 2.298097038856279806 ) ) ;
#1264 = LINE ( 'NONE', #10854, #1135 ) ;
#1265 = PLANE ( 'NONE',  #4606 ) ;
#1266 = CIRCLE ( 'NONE', #8214, 100.0000000000000284 ) ;
#1267 = ORIENTED_EDGE ( 'NONE', *, *, #6550, .T. ) ;
#1268 = DIRECTION ( 'NONE',  ( -0.000000000000000000, -1.000000000000000000, -0.000000000000000000 ) ) ;
#1269 = CARTESIAN_POINT ( 'NONE',  ( 71.40110041870237012, 15.97341095676601697, 23.12535642331794605 ) ) ;
#1270 = ORIENTED_EDGE ( 'NONE', *, *, #7421, .F. ) ;
#1271 = CYLINDRICAL_SURFACE ( 'NONE', #5282, 10.00000000000000178 ) ;
#1272 = AXIS2_PLACEMENT_3D ( 'NONE', #6702, #7511, #788 ) ;
#1273 = VECTOR ( 'NONE', #6369, 1000.000000000000000 ) ;
#1274 = ORIENTED_EDGE ( 'NONE', *, *, #3107, .T. ) ;
#1275 = PRODUCT_DEFINITION_CONTEXT ( 'detailed design', #10350, 'design' ) ;
#1276 = CARTESIAN_POINT ( 'NONE',  ( 2.500000000000000000, 0.000000000000000000, 0.000000000000000000 ) ) ;
#1277 = CARTESIAN_POINT ( 'NONE',  ( 1.990051048614449116E-16, 110.2500000000000000, 3.250000000000000444 ) ) ;
#1278 = VERTEX_POINT ( 'NONE', #2755 ) ;
#1279 = ADVANCED_FACE ( 'NONE', ( #5699 ), #5517, .T. ) ;
#1280 = CARTESIAN_POINT ( 'NONE',  ( -100.7495955565347288, 275.0000000000000000, 29.57226733266632124 ) ) ;
#1281 = FACE_OUTER_BOUND ( 'NONE', #7568, .T. ) ;
#1282 = EDGE_CURVE ( 'NONE', #5525, #2631, #11841, .T. ) ;
#1283 = DIRECTION ( 'NONE',  ( 0.000000000000000000, 1.000000000000000000, 0.000000000000000000 ) ) ;
#1284 = VECTOR ( 'NONE', #579, 1000.000000000000000 ) ;
#1285 = AXIS2_PLACEMENT_3D ( 'NONE', #870, #2729, #748 ) ;
#1286 = ORIENTED_EDGE ( 'NONE', *, *, #1936, .F. ) ;
#1287 = CARTESIAN_POINT ( 'NONE',  ( -25.00000000000000000, 570.2996408614167194, -29.99999999999999289 ) ) ;
#1288 = EDGE_CURVE ( 'NONE', #6190, #9044, #12187, .T. ) ;
#1289 = DIRECTION ( 'NONE',  ( -0.2499999999999996947, 0.000000000000000000, -0.9682458365518543664 ) ) ;
#1290 = DIRECTION ( 'NONE',  ( 0.000000000000000000, 0.000000000000000000, 1.000000000000000000 ) ) ;
#1291 = VECTOR ( 'NONE', #3516, 1000.000000000000114 ) ;
#1292 = DIRECTION ( 'NONE',  ( 1.000000000000000000, 0.000000000000000000, -0.000000000000000000 ) ) ;
#1293 = CARTESIAN_POINT ( 'NONE',  ( -45.35898384862240107, 67.00000000000008527, 25.98076211353315657 ) ) ;
#1294 = CARTESIAN_POINT ( 'NONE',  ( -28.72281323269012532, 77.00000000000000000, 8.660254037844445918 ) ) ;
#1295 = CARTESIAN_POINT ( 'NONE',  ( -1.915364268218909150, 111.6874999986344079, 1.915364268218909594 ) ) ;
#1296 = ORIENTED_EDGE ( 'NONE', *, *, #10352, .T. ) ;
#1297 = LINE ( 'NONE', #10769, #9355 ) ;
#1298 = VECTOR ( 'NONE', #12093, 1000.000000000000000 ) ;
#1299 = AXIS2_PLACEMENT_3D ( 'NONE', #3317, #5313, #9091 ) ;
#1300 = B_SPLINE_CURVE_WITH_KNOTS ( 'NONE', 3,
 ( #180, #7730, #11608, #4735 ),
 .UNSPECIFIED., .F., .F.,
 ( 4, 4 ),
 ( 0.0009573067811866411980, 0.001207306781186544276 ),
 .UNSPECIFIED. ) ;
#1301 = EDGE_CURVE ( 'NONE', #5989, #7101, #10232, .T. ) ;
#1302 = ADVANCED_FACE ( 'NONE', ( #6689 ), #4871, .F. ) ;
#1303 = ORIENTED_EDGE ( 'NONE', *, *, #5273, .F. ) ;
#1304 = CARTESIAN_POINT ( 'NONE',  ( 0.000000000000000000, 87.50000000000000000, 0.000000000000000000 ) ) ;
#1305 = ORIENTED_EDGE ( 'NONE', *, *, #4806, .T. ) ;
#1306 = DIRECTION ( 'NONE',  ( -0.000000000000000000, -1.000000000000000000, -0.000000000000000000 ) ) ;
#1307 = CARTESIAN_POINT ( 'NONE',  ( 30.00100000000000122, 77.00000000000000000, 8.660254037844445918 ) ) ;
#1308 = ORIENTED_EDGE ( 'NONE', *, *, #354, .F. ) ;
#1309 = VECTOR ( 'NONE', #6876, 1000.000000000000000 ) ;
#1310 = DIRECTION ( 'NONE',  ( 0.000000000000000000, 1.000000000000000000, 0.000000000000000000 ) ) ;
#1311 = DIRECTION ( 'NONE',  ( 0.000000000000000000, 0.000000000000000000, 1.000000000000000000 ) ) ;
#1312 = VERTEX_POINT ( 'NONE', #316 ) ;
#1313 = CLOSED_SHELL ( 'NONE', ( #3230, #7953, #9387, #12328, #9620, #5138, #7591, #4251, #2390, #5665, #9897, #798, #10427, #12260, #12222, #2538, #10180, #10873, #5121, #9944, #12231, #11960, #6025, #4909, #4674, #5505, #5178, #3185, #9915 ) ) ;
#1314 = CARTESIAN_POINT ( 'NONE',  ( -1.915364268218909150, 111.6874999986344079, 1.915364268218909594 ) ) ;
#1315 = CIRCLE ( 'NONE', #5902, 35.00000000000000000 ) ;
#1316 = VECTOR ( 'NONE', #3519, 1000.000000000000000 ) ;
#1317 = ORIENTED_EDGE ( 'NONE', *, *, #9120, .T. ) ;
#1318 = DIRECTION ( 'NONE',  ( 0.000000000000000000, 0.000000000000000000, 1.000000000000000000 ) ) ;
#1319 = DIRECTION ( 'NONE',  ( 0.000000000000000000, 0.000000000000000000, 1.000000000000000000 ) ) ;
#1320 = ORIENTED_EDGE ( 'NONE', *, *, #2719, .F. ) ;
#1321 = COLOUR_RGB ( '', 0.66274510, 0.83137255, 0.94901961) ;
#1322 = DIRECTION ( 'NONE',  ( 0.8660254037844394848, -0.4999999999999985567, 0.000000000000000000 ) ) ;
#1323 = CARTESIAN_POINT ( 'NONE',  ( 0.000000000000000000, 110.0000000000000000, 0.000000000000000000 ) ) ;
#1324 = ORIENTED_EDGE ( 'NONE', *, *, #3762, .F. ) ;
#1325 = CYLINDRICAL_SURFACE ( 'NONE', #1672, 95.00000000000002842 ) ;
#1326 = LINE ( 'NONE', #8101, #11490 ) ;
#1327 = CARTESIAN_POINT ( 'NONE',  ( 121.4644660940682428, 46.46446609406732620, -20.00000000000000000 ) ) ;
#1328 = EDGE_LOOP ( 'NONE', ( #4671, #5895, #9361, #10082, #6793 ) ) ;
#1329 = CARTESIAN_POINT ( 'NONE',  ( 165.0000000000011369, 225.0000000000000853, -20.00000000000000000 ) ) ;
#1330 = EDGE_CURVE ( 'NONE', #7513, #6899, #8632, .T. ) ;
#1331 = CARTESIAN_POINT ( 'NONE',  ( 71.99568681135517068, 14.96114988300740656, 21.09760594592229310 ) ) ;
#1332 = VECTOR ( 'NONE', #9870, 1000.000000000000227 ) ;
#1333 = EDGE_CURVE ( 'NONE', #11288, #6005, #8038, .T. ) ;
#1334 = ORIENTED_EDGE ( 'NONE', *, *, #9809, .T. ) ;
#1335 = FACE_BOUND ( 'NONE', #4548, .T. ) ;
#1336 = CARTESIAN_POINT ( 'NONE',  ( 70.79540202493410561, 40.42529689935005877, -24.98706380095369894 ) ) ;
#1337 = ORIENTED_EDGE ( 'NONE', *, *, #10508, .F. ) ;
#1338 = DIRECTION ( 'NONE',  ( 0.000000000000000000, 1.000000000000000000, 0.000000000000000000 ) ) ;
#1339 = CARTESIAN_POINT ( 'NONE',  ( 71.78382695943244585, 49.48706010510388609, 21.72958296927689759 ) ) ;
#1340 = VERTEX_POINT ( 'NONE', #2135 ) ;
#1341 = LINE ( 'NONE', #8869, #1050 ) ;
#1342 = VECTOR ( 'NONE', #10158, 1000.000000000000114 ) ;
#1343 = CARTESIAN_POINT ( 'NONE',  ( 0.000000000000000000, 67.00000000000000000, 0.000000000000000000 ) ) ;
#1344 = CARTESIAN_POINT ( 'NONE',  ( 0.000000000000000000, 110.0000000000000000, 0.000000000000000000 ) ) ;
#1345 = EDGE_CURVE ( 'NONE', #11537, #3527, #3608, .T. ) ;
#1346 = ORIENTED_EDGE ( 'NONE', *, *, #5064, .F. ) ;
#1347 = SURFACE_SIDE_STYLE ('',( #4211 ) ) ;
#1348 = EDGE_LOOP ( 'NONE', ( #9516, #8341, #6017, #6615, #423 ) ) ;
#1349 = CARTESIAN_POINT ( 'NONE',  ( 10.19254911989230727, 36.28349364905406560, 80.00000000000000000 ) ) ;
#1350 = CARTESIAN_POINT ( 'NONE',  ( 2.500000000000000000, 0.000000000000000000, 0.000000000000000000 ) ) ;
#1351 = DIRECTION ( 'NONE',  ( 0.000000000000000000, 0.000000000000000000, -1.000000000000000000 ) ) ;
#1352 = DIRECTION ( 'NONE',  ( 0.000000000000000000, 1.000000000000000000, -0.000000000000000000 ) ) ;
#1353 = CARTESIAN_POINT ( 'NONE',  ( -0.5177535225088374382, 44.99389217799025431, 75.00000000000001421 ) ) ;
#1354 = DIRECTION ( 'NONE',  ( 0.000000000000000000, 1.000000000000000000, 0.000000000000000000 ) ) ;
#1355 = CARTESIAN_POINT ( 'NONE',  ( -2.708734125000000326, 111.7499999986344079, 1.121994411437818862 ) ) ;
#1356 = ORIENTED_EDGE ( 'NONE', *, *, #7015, .F. ) ;
#1357 = CARTESIAN_POINT ( 'NONE',  ( 0.000000000000000000, 165.0000000000000000, 0.000000000000000000 ) ) ;
#1358 = ADVANCED_FACE ( 'NONE', ( #5003 ), #256, .T. ) ;
#1359 = VECTOR ( 'NONE', #1537, 1000.000000000000000 ) ;
#1360 =( GEOMETRIC_REPRESENTATION_CONTEXT ( 3 ) GLOBAL_UNCERTAINTY_ASSIGNED_CONTEXT ( ( #9114 ) ) GLOBAL_UNIT_ASSIGNED_CONTEXT ( ( #3339, #10754, #4149 ) ) REPRESENTATION_CONTEXT ( 'NONE', 'WORKASPACE' ) );
#1361 = ORIENTED_EDGE ( 'NONE', *, *, #4938, .F. ) ;
#1362 = DIRECTION ( 'NONE',  ( -0.000000000000000000, -0.000000000000000000, 1.000000000000000000 ) ) ;
#1363 = EDGE_LOOP ( 'NONE', ( #3842, #1356, #12095, #9800 ) ) ;
#1364 = CARTESIAN_POINT ( 'NONE',  ( 34.73110591274434000, 77.00000000000000000, -8.660254037844445918 ) ) ;
#1365 = PLANE ( 'NONE',  #6497 ) ;
#1366 = ORIENTED_EDGE ( 'NONE', *, *, #8545, .T. ) ;
#1367 = DIRECTION ( 'NONE',  ( 1.000000000000000000, -0.000000000000000000, 0.000000000000000000 ) ) ;
#1368 = CARTESIAN_POINT ( 'NONE',  ( -29.32777202433393526, 87.43477800909944619, -9.413311639618301641 ) ) ;
#1369 = ADVANCED_FACE ( 'NONE', ( #7680 ), #10727, .F. ) ;
#1370 = EDGE_CURVE ( 'NONE', #11096, #11491, #11678, .T. ) ;
#1371 = AXIS2_PLACEMENT_3D ( 'NONE', #3501, #10283, #4615 ) ;
#1372 = VERTEX_POINT ( 'NONE', #4943 ) ;
#1373 = CARTESIAN_POINT ( 'NONE',  ( 70.40708232491709850, 46.56656424045070253, -25.84664880093518136 ) ) ;
#1374 = VERTEX_POINT ( 'NONE', #8728 ) ;
#1375 = CARTESIAN_POINT ( 'NONE',  ( 1.734723475976807094E-14, 65.00000000000000000, 57.08203932499370836 ) ) ;
#1376 = CARTESIAN_POINT ( 'NONE',  ( 125.0000000000009663, 42.92893218813457423, 20.00000000000000000 ) ) ;
#1377 = EDGE_CURVE ( 'NONE', #8030, #8106, #3017, .T. ) ;
#1378 = ORIENTED_EDGE ( 'NONE', *, *, #3887, .F. ) ;
#1379 = DIRECTION ( 'NONE',  ( 1.000000000000000000, 0.000000000000000000, 0.000000000000000000 ) ) ;
#1380 = DIRECTION ( 'NONE',  ( 0.000000000000000000, 0.000000000000000000, 1.000000000000000000 ) ) ;
#1381 = ORIENTED_EDGE ( 'NONE', *, *, #10829, .T. ) ;
#1382 = DIRECTION ( 'NONE',  ( 3.469446951953613203E-16, 0.000000000000000000, -1.000000000000000000 ) ) ;
#1383 = CARTESIAN_POINT ( 'NONE',  ( 74.31677170407374433, 41.41979450890040937, -24.80746953044373981 ) ) ;
#1384 = CARTESIAN_POINT ( 'NONE',  ( 74.16198487095664404, 40.00000000000009237, 29.99999999999999645 ) ) ;
#1385 = ORIENTED_EDGE ( 'NONE', *, *, #643, .T. ) ;
#1386 = CARTESIAN_POINT ( 'NONE',  ( 28.72281323269012532, 87.00000000000000000, 8.660254037844435260 ) ) ;
#1387 = CARTESIAN_POINT ( 'NONE',  ( 69.57792926911190534, 18.32862386349516015, 27.99850680361992517 ) ) ;
#1388 = CIRCLE ( 'NONE', #8934, 5.000000000000000888 ) ;
#1389 = VECTOR ( 'NONE', #6685, 1000.000000000000000 ) ;
#1390 = EDGE_LOOP ( 'NONE', ( #3549, #192, #5200, #5928 ) ) ;
#1391 = CARTESIAN_POINT ( 'NONE',  ( 72.28000013808933488, 45.16202677360365669, -20.04822706562131884 ) ) ;
#1392 = DIRECTION ( 'NONE',  ( 0.000000000000000000, 0.000000000000000000, 1.000000000000000000 ) ) ;
#1393 = ORIENTED_EDGE ( 'NONE', *, *, #5864, .F. ) ;
#1394 = ADVANCED_FACE ( 'NONE', ( #3128 ), #9173, .T. ) ;
#1395 = CARTESIAN_POINT ( 'NONE',  ( 3.249999999999999556, 110.9375000000000000, -1.346194077712561166 ) ) ;
#1396 = EDGE_CURVE ( 'NONE', #11537, #1374, #6932, .T. ) ;
#1397 = CARTESIAN_POINT ( 'NONE',  ( 75.14265900998388759, 43.33802077090974336, 23.72616954495132191 ) ) ;
#1398 = ORIENTED_EDGE ( 'NONE', *, *, #4341, .T. ) ;
#1399 = CARTESIAN_POINT ( 'NONE',  ( 45.35898384862240107, 5.499999999999840128, 9.526279441628638267 ) ) ;
#1400 = AXIS2_PLACEMENT_3D ( 'NONE', #6661, #1798, #8459 ) ;
#1401 = LINE ( 'NONE', #336, #3404 ) ;
#1402 = DIRECTION ( 'NONE',  ( 0.000000000000000000, 0.000000000000000000, 1.000000000000000000 ) ) ;
#1403 = CARTESIAN_POINT ( 'NONE',  ( -12.32411137850302119, 23.28349364905396612, 79.50000000000000000 ) ) ;
#1404 = ADVANCED_FACE ( 'NONE', ( #2247 ), #2946, .T. ) ;
#1405 = EDGE_LOOP ( 'NONE', ( #115, #8358 ) ) ;
#1406 = ORIENTED_EDGE ( 'NONE', *, *, #9688, .F. ) ;
#1407 = ORIENTED_EDGE ( 'NONE', *, *, #9808, .F. ) ;
#1408 = VECTOR ( 'NONE', #8580, 1000.000000000000000 ) ;
#1409 = AXIS2_PLACEMENT_3D ( 'NONE', #11572, #5209, #459 ) ;
#1410 = CARTESIAN_POINT ( 'NONE',  ( 0.000000000000000000, 340.0000000000000000, 0.000000000000000000 ) ) ;
#1411 = DIRECTION ( 'NONE',  ( 0.000000000000000000, 1.000000000000000000, -1.224646799147353207E-16 ) ) ;
#1412 = FACE_OUTER_BOUND ( 'NONE', #3481, .T. ) ;
#1413 = CARTESIAN_POINT ( 'NONE',  ( 30.00100000000000122, 87.00000000000000000, -8.660254037844435260 ) ) ;
#1414 = CIRCLE ( 'NONE', #5603, 22.00000000000000355 ) ;
#1415 = CARTESIAN_POINT ( 'NONE',  ( 33.79339916392899568, 75.30908861350523864, -7.588998470350058589 ) ) ;
#1416 = VECTOR ( 'NONE', #6438, 1000.000000000000000 ) ;
#1417 = CARTESIAN_POINT ( 'NONE',  ( 0.000000000000000000, 165.0000000000000000, -9.999999999999998224 ) ) ;
#1418 = CARTESIAN_POINT ( 'NONE',  ( 71.22405252493085470, 11.35584875400091320, -23.50371070993386624 ) ) ;
#1419 = CARTESIAN_POINT ( 'NONE',  ( -1.915364268218909150, 113.6874999986344079, 1.915364268218909594 ) ) ;
#1420 = VERTEX_POINT ( 'NONE', #10544 ) ;
#1421 = CARTESIAN_POINT ( 'NONE',  ( -7.907287480251421030, 41.13333024919781167, 80.00000000000000000 ) ) ;
#1422 = VECTOR ( 'NONE', #9629, 1000.000000000000000 ) ;
#1423 = AXIS2_PLACEMENT_3D ( 'NONE', #949, #4556, #8530 ) ;
#1424 = ORIENTED_EDGE ( 'NONE', *, *, #5390, .T. ) ;
#1425 = DIRECTION ( 'NONE',  ( 0.000000000000000000, 0.000000000000000000, 1.000000000000000000 ) ) ;
#1426 = ORIENTED_EDGE ( 'NONE', *, *, #1301, .F. ) ;
#1427 = DIRECTION ( 'NONE',  ( 0.000000000000000000, 1.000000000000000000, 0.000000000000000000 ) ) ;
#1428 = CARTESIAN_POINT ( 'NONE',  ( 74.31403689601799556, 18.59282065414787510, -24.81089180822486639 ) ) ;
#1429 = VERTEX_POINT ( 'NONE', #5998 ) ;
#1430 = AXIS2_PLACEMENT_3D ( 'NONE', #10005, #3409, #12081 ) ;
#1431 = EDGE_CURVE ( 'NONE', #1372, #1941, #9785, .T. ) ;
#1432 = LINE ( 'NONE', #10900, #5872 ) ;
#1433 = ADVANCED_FACE ( 'NONE', ( #1260 ), #5070, .T. ) ;
#1434 = CIRCLE ( 'NONE', #8184, 2.041999999999999815 ) ;
#1435 = DIRECTION ( 'NONE',  ( -0.000000000000000000, -1.000000000000000000, -0.000000000000000000 ) ) ;
#1436 = ORIENTED_EDGE ( 'NONE', *, *, #4623, .T. ) ;
#1437 = CARTESIAN_POINT ( 'NONE',  ( 0.000000000000000000, 67.00000000000000000, 0.000000000000000000 ) ) ;
#1438 = VERTEX_POINT ( 'NONE', #130 ) ;
#1439 = LINE ( 'NONE', #11859, #12313 ) ;
#1440 = CARTESIAN_POINT ( 'NONE',  ( 0.000000000000000000, 75.00000000000001421, 0.000000000000000000 ) ) ;
#1441 = EDGE_CURVE ( 'NONE', #7734, #7317, #3067, .T. ) ;
#1442 = VERTEX_POINT ( 'NONE', #3007 ) ;
#1443 = CARTESIAN_POINT ( 'NONE',  ( 0.000000000000000000, 127.0000000000000000, 0.000000000000000000 ) ) ;
#1444 = CARTESIAN_POINT ( 'NONE',  ( 3.592712519748450628, 38.78525403784453118, 79.50000000000000000 ) ) ;
#1445 = ORIENTED_EDGE ( 'NONE', *, *, #1071, .F. ) ;
#1446 = ADVANCED_FACE ( 'NONE', ( #6811 ), #2071, .T. ) ;
#1447 = DIRECTION ( 'NONE',  ( -0.000000000000000000, 1.000000000000000000, -0.000000000000000000 ) ) ;
#1448 = CARTESIAN_POINT ( 'NONE',  ( -30.55518048406710818, 80.37544454677752981, -1.186187415305626436 ) ) ;
#1449 = DIRECTION ( 'NONE',  ( 0.000000000000000000, 0.000000000000000000, -1.000000000000000000 ) ) ;
#1450 = ORIENTED_EDGE ( 'NONE', *, *, #3823, .T. ) ;
#1451 = CIRCLE ( 'NONE', #2047, 2.041999999999999815 ) ;
#1452 = CARTESIAN_POINT ( 'NONE',  ( 74.77359728361332714, 17.31486177643626334, 24.22100760279318621 ) ) ;
#1453 = ORIENTED_EDGE ( 'NONE', *, *, #9437, .F. ) ;
#1454 = EDGE_CURVE ( 'NONE', #7484, #7525, #4811, .T. ) ;
#1455 = CARTESIAN_POINT ( 'NONE',  ( 72.29554967163204537, 49.93605735591993522, -19.96827991394273383 ) ) ;
#1456 = EDGE_CURVE ( 'NONE', #2323, #9195, #9966, .T. ) ;
#1457 = DIRECTION ( 'NONE',  ( 1.000000000000000000, -1.387778780781445676E-14, 0.000000000000000000 ) ) ;
#1458 = ORIENTED_EDGE ( 'NONE', *, *, #7606, .F. ) ;
#1459 = CARTESIAN_POINT ( 'NONE',  ( 1.990051048614449116E-16, 111.2500000000000000, 3.250000000000000444 ) ) ;
#1460 = CARTESIAN_POINT ( 'NONE',  ( 74.38206444891756064, 41.64350558143038228, 24.72514820121040557 ) ) ;
#1461 = AXIS2_PLACEMENT_3D ( 'NONE', #1376, #1564, #4301 ) ;
#1462 = ORIENTED_EDGE ( 'NONE', *, *, #11573, .T. ) ;
#1463 = CARTESIAN_POINT ( 'NONE',  ( 1.990051048614449116E-16, 113.1249999972688158, 3.250000000000000444 ) ) ;
#1464 = PLANE ( 'NONE',  #3000 ) ;
#1465 = DIRECTION ( 'NONE',  ( -0.000000000000000000, -0.000000000000000000, 1.000000000000000000 ) ) ;
#1466 = CARTESIAN_POINT ( 'NONE',  ( -1.915364268218909150, 112.6874999986344079, 1.915364268218909594 ) ) ;
#1467 = EDGE_LOOP ( 'NONE', ( #12126, #5840 ) ) ;
#1468 = VERTEX_POINT ( 'NONE', #5433 ) ;
#1469 = SURFACE_STYLE_USAGE ( .BOTH. , #10878 ) ;
#1470 = ORIENTED_EDGE ( 'NONE', *, *, #2038, .T. ) ;
#1471 = AXIS2_PLACEMENT_3D ( 'NONE', #2725, #1790, #9382 ) ;
#1472 = CARTESIAN_POINT ( 'NONE',  ( 0.000000000000000000, 77.00000000000000000, 0.000000000000000000 ) ) ;
#1473 = DIRECTION ( 'NONE',  ( 0.000000000000000000, -1.000000000000000000, 0.000000000000000000 ) ) ;
#1474 = DIRECTION ( 'NONE',  ( -1.000000000000000000, -0.000000000000000000, -0.000000000000000000 ) ) ;
#1475 = DIRECTION ( 'NONE',  ( -0.000000000000000000, -1.000000000000000000, -0.000000000000000000 ) ) ;
#1476 = DIRECTION ( 'NONE',  ( 0.000000000000000000, 0.000000000000000000, 1.000000000000000000 ) ) ;
#1477 = FACE_OUTER_BOUND ( 'NONE', #4787, .T. ) ;
#1478 = DIRECTION ( 'NONE',  ( 0.000000000000000000, 0.000000000000000000, 1.000000000000000000 ) ) ;
#1479 = AXIS2_PLACEMENT_3D ( 'NONE', #1276, #4080, #6823 ) ;
#1480 = CARTESIAN_POINT ( 'NONE',  ( 8.572527594031472993E-15, 63.00000000000000000, -70.00000000000000000 ) ) ;
#1481 = CARTESIAN_POINT ( 'NONE',  ( 2.708734124999999882, 113.2499999986344079, -1.121994411437820638 ) ) ;
#1482 = CARTESIAN_POINT ( 'NONE',  ( 69.85388127645425982, 75.26794919243111792, -7.660254037844449471 ) ) ;
#1483 = ADVANCED_FACE ( 'NONE', ( #11922 ), #11863, .F. ) ;
#1484 = AXIS2_PLACEMENT_3D ( 'NONE', #3606, #1556, #5359 ) ;
#1485 = EDGE_LOOP ( 'NONE', ( #5479, #1619 ) ) ;
#1486 = CARTESIAN_POINT ( 'NONE',  ( 31.88521078284829713, 87.00000000000001421, 14.43375672974067569 ) ) ;
#1487 = ORIENTED_EDGE ( 'NONE', *, *, #4666, .F. ) ;
#1488 = CARTESIAN_POINT ( 'NONE',  ( 0.000000000000000000, 345.0000000000000568, -59.99999999999999289 ) ) ;
#1489 = FACE_OUTER_BOUND ( 'NONE', #2859, .T. ) ;
#1490 = ORIENTED_EDGE ( 'NONE', *, *, #5036, .F. ) ;
#1491 = CARTESIAN_POINT ( 'NONE',  ( 165.0000000000011369, 30.00000000000008882, -19.99999999999999645 ) ) ;
#1492 = DIRECTION ( 'NONE',  ( 1.000000000000000000, 0.000000000000000000, -0.000000000000000000 ) ) ;
#1493 = CONTEXT_DEPENDENT_SHAPE_REPRESENTATION ( #10181, #2205 ) ;
#1494 = VECTOR ( 'NONE', #6669, 1000.000000000000000 ) ;
#1495 = ORIENTED_EDGE ( 'NONE', *, *, #3254, .F. ) ;
#1496 = DIRECTION ( 'NONE',  ( 0.000000000000000000, 0.000000000000000000, 1.000000000000000000 ) ) ;
#1497 = AXIS2_PLACEMENT_3D ( 'NONE', #7319, #7066, #11118 ) ;
#1498 = EDGE_CURVE ( 'NONE', #5994, #10814, #4603, .T. ) ;
#1499 = EDGE_CURVE ( 'NONE', #9385, #11869, #4012, .T. ) ;
#1500 = VERTEX_POINT ( 'NONE', #6365 ) ;
#1501 = DIRECTION ( 'NONE',  ( -0.000000000000000000, 1.000000000000000000, -0.000000000000000000 ) ) ;
#1502 = PLANE ( 'NONE',  #9393 ) ;
#1503 = EDGE_LOOP ( 'NONE', ( #8693, #4343, #10905, #836 ) ) ;
#1504 = VECTOR ( 'NONE', #2164, 1000.000000000000000 ) ;
#1505 = ORIENTED_EDGE ( 'NONE', *, *, #10254, .F. ) ;
#1506 = CARTESIAN_POINT ( 'NONE',  ( 3.592712519748450628, 38.78525403784453118, 80.00000000000000000 ) ) ;
#1507 = DIRECTION ( 'NONE',  ( -1.000000000000000000, 0.000000000000000000, -1.224646799147352961E-16 ) ) ;
#1508 = ORIENTED_EDGE ( 'NONE', *, *, #4461, .F. ) ;
#1509 = DIRECTION ( 'NONE',  ( -1.000000000000000000, 0.000000000000000000, -0.000000000000000000 ) ) ;
#1510 = DIRECTION ( 'NONE',  ( 0.000000000000000000, -0.4999999999999976130, -0.8660254037844400399 ) ) ;
#1511 = CARTESIAN_POINT ( 'NONE',  ( -6.407287480251453893, 38.53525403784446723, 79.50000000000000000 ) ) ;
#1512 = ORIENTED_EDGE ( 'NONE', *, *, #8707, .F. ) ;
#1513 = CARTESIAN_POINT ( 'NONE',  ( 28.47250777504872588, 87.47929846073044757, 9.490423323819145551 ) ) ;
#1514 = CARTESIAN_POINT ( 'NONE',  ( 75.13748311126856549, 16.66004759637138832, 23.73500236558975729 ) ) ;
#1515 = ADVANCED_FACE ( 'NONE', ( #5310 ), #6119, .F. ) ;
#1516 = EDGE_CURVE ( 'NONE', #9990, #4918, #10969, .T. ) ;
#1517 = VECTOR ( 'NONE', #3348, 1000.000000000000000 ) ;
#1518 = VERTEX_POINT ( 'NONE', #9150 ) ;
#1519 = CARTESIAN_POINT ( 'NONE',  ( 72.61843774138908714, 50.00000000000009237, -18.75000000000000355 ) ) ;
#1520 = DIRECTION ( 'NONE',  ( 0.000000000000000000, 0.000000000000000000, 1.000000000000000000 ) ) ;
#1521 = VERTEX_POINT ( 'NONE', #1506 ) ;
#1522 = B_SPLINE_CURVE_WITH_KNOTS ( 'NONE', 3,
 ( #9804, #4141, #7131, #6078 ),
 .UNSPECIFIED., .F., .F.,
 ( 4, 4 ),
 ( 0.0002502309401078863893, 0.0005002309401076776314 ),
 .UNSPECIFIED. ) ;
#1523 = CARTESIAN_POINT ( 'NONE',  ( 5.092712519748611832, 18.61666975080242992, 79.50000000000000000 ) ) ;
#1524 = CARTESIAN_POINT ( 'NONE',  ( 76.01396467472481788, 44.35825346231943200, 22.47201498426101196 ) ) ;
#1525 = ORIENTED_EDGE ( 'NONE', *, *, #2688, .T. ) ;
#1526 = DIRECTION ( 'NONE',  ( 0.000000000000000000, 1.000000000000000000, 0.000000000000000000 ) ) ;
#1527 = FILL_AREA_STYLE ('',( #4321 ) ) ;
#1528 = CARTESIAN_POINT ( 'NONE',  ( -1.915364268218909816, 111.9374999986344079, -1.915364268218909150 ) ) ;
#1529 = VECTOR ( 'NONE', #7637, 1000.000000000000000 ) ;
#1530 = ADVANCED_FACE ( 'NONE', ( #7304 ), #7973, .T. ) ;
#1531 = ORIENTED_EDGE ( 'NONE', *, *, #9964, .T. ) ;
#1532 =( LENGTH_UNIT ( ) NAMED_UNIT ( * ) SI_UNIT ( .MILLI., .METRE. ) );
#1533 = ORIENTED_EDGE ( 'NONE', *, *, #1370, .T. ) ;
#1534 = UNCERTAINTY_MEASURE_WITH_UNIT (LENGTH_MEASURE( 1.000000000000000082E-05 ), #1039, 'distance_accuracy_value', 'NONE');
#1535 = CIRCLE ( 'NONE', #2530, 17.00000000000000000 ) ;
#1536 = DIRECTION ( 'NONE',  ( -0.000000000000000000, -0.000000000000000000, -1.000000000000000000 ) ) ;
#1537 = DIRECTION ( 'NONE',  ( -0.000000000000000000, 1.000000000000000000, -0.000000000000000000 ) ) ;
#1538 = CARTESIAN_POINT ( 'NONE',  ( -31.92904760676809062, 76.99999999999998579, 7.658217335466646070 ) ) ;
#1539 = DIRECTION ( 'NONE',  ( 7.011174048739587977E-15, 1.000000000000000000, 0.000000000000000000 ) ) ;
#1540 = CARTESIAN_POINT ( 'NONE',  ( -14.19078112930532853, 30.25000000000008882, 80.00000000000000000 ) ) ;
#1541 = DIRECTION ( 'NONE',  ( 0.000000000000000000, 0.000000000000000000, 1.000000000000000000 ) ) ;
#1542 = PLANE ( 'NONE',  #3430 ) ;
#1543 = CARTESIAN_POINT ( 'NONE',  ( 69.55111042745876659, 18.70063303202293170, -28.06526308249821966 ) ) ;
#1544 = CARTESIAN_POINT ( 'NONE',  ( -2.298097038856279362, 112.3750000000000000, 2.298097038856279806 ) ) ;
#1545 = CARTESIAN_POINT ( 'NONE',  ( 2.708734124999999882, 110.6249999986343937, 1.121994411437819084 ) ) ;
#1546 = DIRECTION ( 'NONE',  ( 0.000000000000000000, 1.000000000000000000, -1.287488025362403787E-15 ) ) ;
#1547 = CARTESIAN_POINT ( 'NONE',  ( 3.249999999999999556, 112.8124999972687874, -1.346194077712561166 ) ) ;
#1548 = ORIENTED_EDGE ( 'NONE', *, *, #4290, .T. ) ;
#1549 = CARTESIAN_POINT ( 'NONE',  ( 5.092712519748452848, 41.38333024919784719, 79.50000000000000000 ) ) ;
#1550 = VERTEX_POINT ( 'NONE', #9028 ) ;
#1551 = EDGE_CURVE ( 'NONE', #5535, #9044, #6178, .T. ) ;
#1552 = CARTESIAN_POINT ( 'NONE',  ( -7.907287480251413925, 18.86666975080236597, 80.00000000000000000 ) ) ;
#1553 = ADVANCED_FACE ( 'NONE', ( #4241 ), #8097, .F. ) ;
#1554 = DIRECTION ( 'NONE',  ( 0.000000000000000000, 1.000000000000000000, 0.000000000000000000 ) ) ;
#1555 = EDGE_LOOP ( 'NONE', ( #9556, #567, #3671, #10469, #7819, #2628, #1688, #11556, #2618, #8107 ) ) ;
#1556 = DIRECTION ( 'NONE',  ( 0.7071067811865495711, 0.7071067811865455743, 0.000000000000000000 ) ) ;
#1557 = CARTESIAN_POINT ( 'NONE',  ( -28.14852131675075242, 87.98519278820045031, -10.36665800225805967 ) ) ;
#1558 = ADVANCED_FACE ( 'NONE', ( #11038 ), #221, .T. ) ;
#1559 = ORIENTED_EDGE ( 'NONE', *, *, #6927, .F. ) ;
#1560 = CARTESIAN_POINT ( 'NONE',  ( 69.55717041450675708, 41.30413405089374379, -28.04997484771492822 ) ) ;
#1561 = VECTOR ( 'NONE', #11409, 1000.000000000000000 ) ;
#1562 = ORIENTED_EDGE ( 'NONE', *, *, #3432, .T. ) ;
#1563 = CARTESIAN_POINT ( 'NONE',  ( -1.190781129305471087, 30.00000000000008882, 65.00000000000000000 ) ) ;
#1564 = DIRECTION ( 'NONE',  ( -0.7071067811865503483, -0.7071067811865447972, 0.000000000000000000 ) ) ;
#1565 = ORIENTED_EDGE ( 'NONE', *, *, #10964, .F. ) ;
#1566 = DIRECTION ( 'NONE',  ( -0.4999999999999942268, 0.8660254037844419273, 0.000000000000000000 ) ) ;
#1567 = PLANE ( 'NONE',  #10870 ) ;
#1568 = AXIS2_PLACEMENT_3D ( 'NONE', #1776, #5529, #7332 ) ;
#1569 = VERTEX_POINT ( 'NONE', #3245 ) ;
#1570 = AXIS2_PLACEMENT_3D ( 'NONE', #1632, #3738, #5436 ) ;
#1571 = CARTESIAN_POINT ( 'NONE',  ( 0.000000000000000000, 0.000000000000000000, 79.50000000000000000 ) ) ;
#1572 = CARTESIAN_POINT ( 'NONE',  ( -20.00000000000000000, 50.00000000000000000, -67.08203932499371547 ) ) ;
#1573 = DIRECTION ( 'NONE',  ( 0.000000000000000000, 0.000000000000000000, -1.000000000000000000 ) ) ;
#1574 = VERTEX_POINT ( 'NONE', #2437 ) ;
#1575 = CARTESIAN_POINT ( 'NONE',  ( -5.970153145843347347E-16, 111.7500000000000000, -3.250000000000000444 ) ) ;
#1576 = LINE ( 'NONE', #1759, #3413 ) ;
#1577 = VERTEX_POINT ( 'NONE', #6242 ) ;
#1578 = DIRECTION ( 'NONE',  ( 3.469446951953613203E-16, 0.000000000000000000, 1.000000000000000000 ) ) ;
#1579 = DIRECTION ( 'NONE',  ( 0.000000000000000000, 0.000000000000000000, 1.000000000000000000 ) ) ;
#1580 = ORIENTED_EDGE ( 'NONE', *, *, #6196, .T. ) ;
#1581 = LINE ( 'NONE', #7381, #11442 ) ;
#1582 = CARTESIAN_POINT ( 'NONE',  ( 74.70253266892970601, 42.54723899285758648, 24.31510929947630117 ) ) ;
#1583 = ORIENTED_EDGE ( 'NONE', *, *, #4955, .T. ) ;
#1584 = DIRECTION ( 'NONE',  ( 0.000000000000000000, 0.000000000000000000, 1.000000000000000000 ) ) ;
#1585 =( GEOMETRIC_REPRESENTATION_CONTEXT ( 3 ) GLOBAL_UNCERTAINTY_ASSIGNED_CONTEXT ( ( #530 ) ) GLOBAL_UNIT_ASSIGNED_CONTEXT ( ( #1165, #7827, #5035 ) ) REPRESENTATION_CONTEXT ( 'NONE', 'WORKASPACE' ) );
#1586 = CARTESIAN_POINT ( 'NONE',  ( 5.525725221640833240, 18.86666975080242992, 79.50000000000000000 ) ) ;
#1587 = CARTESIAN_POINT ( 'NONE',  ( 1.915364268218909594, 112.4374999986344079, 1.915364268218909594 ) ) ;
#1588 = EDGE_CURVE ( 'NONE', #6133, #7105, #5611, .T. ) ;
#1589 = CIRCLE ( 'NONE', #8536, 5.000000000000004441 ) ;
#1590 = CARTESIAN_POINT ( 'NONE',  ( -2.708734124999999882, 112.0624999986344079, 3.317242575922456639E-16 ) ) ;
#1591 = SURFACE_STYLE_USAGE ( .BOTH. , #4385 ) ;
#1592 = CIRCLE ( 'NONE', #2182, 110.0000000000000284 ) ;
#1593 = DIRECTION ( 'NONE',  ( 0.000000000000000000, 1.000000000000000000, 0.000000000000000000 ) ) ;
#1594 = FACE_OUTER_BOUND ( 'NONE', #6328, .T. ) ;
#1595 = EDGE_CURVE ( 'NONE', #2259, #7474, #11789, .T. ) ;
#1596 = DIRECTION ( 'NONE',  ( -1.000000000000000000, -6.938893903907232322E-16, 0.000000000000000000 ) ) ;
#1597 = FACE_OUTER_BOUND ( 'NONE', #1247, .T. ) ;
#1598 = EDGE_CURVE ( 'NONE', #9749, #8477, #6304, .T. ) ;
#1599 = VECTOR ( 'NONE', #1889, 1000.000000000000000 ) ;
#1600 = CARTESIAN_POINT ( 'NONE',  ( -27.56105762898379652, 86.58728811733517716, -11.86287969473305814 ) ) ;
#1601 = DIRECTION ( 'NONE',  ( 1.000000000000000000, -0.000000000000000000, 6.938893903907228378E-17 ) ) ;
#1602 = CARTESIAN_POINT ( 'NONE',  ( 13.37325603157604270, 26.28968282453032757, 73.79828864025962787 ) ) ;
#1603 = CARTESIAN_POINT ( 'NONE',  ( 2.298097038856278918, 111.7499999972688158, -2.298097038856279806 ) ) ;
#1604 = CARTESIAN_POINT ( 'NONE',  ( -2.298097038856279806, 111.6250000000000000, -2.298097038856279362 ) ) ;
#1605 = VECTOR ( 'NONE', #3418, 1000.000000000000114 ) ;
#1606 = DIRECTION ( 'NONE',  ( -0.8660254037844363761, 0.5000000000000038858, 0.000000000000000000 ) ) ;
#1607 = ADVANCED_FACE ( 'NONE', ( #4426 ), #8219, .F. ) ;
#1608 = CARTESIAN_POINT ( 'NONE',  ( 4.953755887175457673, 16.30827223463906250, 74.83741081793274930 ) ) ;
#1609 = ORIENTED_EDGE ( 'NONE', *, *, #3387, .F. ) ;
#1610 = AXIS2_PLACEMENT_3D ( 'NONE', #11271, #10315, #5592 ) ;
#1611 = EDGE_CURVE ( 'NONE', #1631, #10896, #4549, .T. ) ;
#1612 = AXIS2_PLACEMENT_3D ( 'NONE', #9562, #7823, #5032 ) ;
#1613 = CARTESIAN_POINT ( 'NONE',  ( 0.000000000000000000, 2.357898499370431722, -2.818925648462311528E-15 ) ) ;
#1614 = DIRECTION ( 'NONE',  ( 0.000000000000000000, 0.8660254037844405950, 0.4999999999999965028 ) ) ;
#1615 = DIRECTION ( 'NONE',  ( 0.000000000000000000, -1.000000000000000000, 0.000000000000000000 ) ) ;
#1616 = EDGE_LOOP ( 'NONE', ( #272, #10529, #11415, #3957 ) ) ;
#1617 = CARTESIAN_POINT ( 'NONE',  ( 27.96741528345890870, 86.27927944434865992, 11.41192941739706335 ) ) ;
#1618 = DIRECTION ( 'NONE',  ( 0.000000000000000000, 0.000000000000000000, 1.000000000000000000 ) ) ;
#1619 = ORIENTED_EDGE ( 'NONE', *, *, #3254, .T. ) ;
#1620 = CARTESIAN_POINT ( 'NONE',  ( 0.000000000000000000, 285.0000000000000568, 0.000000000000000000 ) ) ;
#1621 = VECTOR ( 'NONE', #9526, 1000.000000000000000 ) ;
#1622 = EDGE_CURVE ( 'NONE', #9381, #8789, #11980, .T. ) ;
#1623 = EDGE_CURVE ( 'NONE', #8974, #12030, #6716, .T. ) ;
#1624 = B_SPLINE_CURVE_WITH_KNOTS ( 'NONE', 3,
 ( #9881, #1353, #5162, #6462, #1727, #3534, #8438, #735, #11270, #6528, #7336, #10313, #10252, #5655, #3471, #8317, #6581, #10122, #9374, #7401, #5533, #9312, #11078, #11136, #9250 ),
 .UNSPECIFIED., .F., .F.,
 ( 4, 2, 1, 2, 2, 2, 2, 2, 2, 2, 2, 2, 4 ),
 ( 0.04461974739530318729, 0.04616436123732098329, 0.04770897507933878623, 0.04925358892135658917, 0.05079820276337438517, 0.05388743044740997717, 0.05543204428942777318, 0.05697665813144557612, 0.06006588581548116812, 0.06315511349951676012, 0.06469972734153456306, 0.06624434118355236600, 0.06933356886758795801 ),
 .UNSPECIFIED. ) ;
#1625 = ORIENTED_EDGE ( 'NONE', *, *, #7141, .T. ) ;
#1626 = CARTESIAN_POINT ( 'NONE',  ( 2.081899558550500280E-15, 122.0000000000000000, -17.00000000000000000 ) ) ;
#1627 = FACE_OUTER_BOUND ( 'NONE', #4261, .T. ) ;
#1628 = EDGE_LOOP ( 'NONE', ( #11303, #10262, #5115, #4111 ) ) ;
#1629 = PLANE ( 'NONE',  #7686 ) ;
#1630 = AXIS2_PLACEMENT_3D ( 'NONE', #2809, #11358, #8265 ) ;
#1631 = VERTEX_POINT ( 'NONE', #4491 ) ;
#1632 = CARTESIAN_POINT ( 'NONE',  ( 0.000000000000000000, 0.000000000000000000, 0.000000000000000000 ) ) ;
#1633 = CARTESIAN_POINT ( 'NONE',  ( 75.00000000000001421, 45.00000000000008527, -19.99999999999999645 ) ) ;
#1634 = CARTESIAN_POINT ( 'NONE',  ( 0.000000000000000000, 75.00000000000000000, -15.00000000000000000 ) ) ;
#1635 = CARTESIAN_POINT ( 'NONE',  ( -0.9407811293052825707, 17.00000000000008882, 79.50000000000000000 ) ) ;
#1636 = EDGE_LOOP ( 'NONE', ( #5230, #2543, #266, #6949 ) ) ;
#1637 = DIRECTION ( 'NONE',  ( 1.224646799147357151E-16, 0.000000000000000000, -1.000000000000000000 ) ) ;
#1638 = DIRECTION ( 'NONE',  ( 0.000000000000000000, 0.000000000000000000, -1.000000000000000000 ) ) ;
#1639 = ADVANCED_FACE ( 'NONE', ( #3915 ), #10515, .T. ) ;
#1640 = EDGE_LOOP ( 'NONE', ( #4892, #782, #4872, #2457 ) ) ;
#1641 = CARTESIAN_POINT ( 'NONE',  ( 2.708734124999999882, 110.5624999986344079, 0.000000000000000000 ) ) ;
#1642 = DIRECTION ( 'NONE',  ( -0.000000000000000000, -1.000000000000000000, -0.000000000000000000 ) ) ;
#1643 =( BOUNDED_CURVE ( )  B_SPLINE_CURVE ( 3, ( #3135, #10732, #5077, #8852 ),
 .UNSPECIFIED., .F., .F. ) 
 B_SPLINE_CURVE_WITH_KNOTS ( ( 4, 4 ),
 ( 1.666086958916892291, 1.694832046014206117 ),
 .UNSPECIFIED. ) 
 CURVE ( )  GEOMETRIC_REPRESENTATION_ITEM ( )  RATIONAL_B_SPLINE_CURVE ( ( 1.000000000000000000, 0.9999311445159493328, 0.9999311445159493328, 1.000000000000000000 ) ) 
 REPRESENTATION_ITEM ( '' )  );
#1644 = ORIENTED_EDGE ( 'NONE', *, *, #9873, .F. ) ;
#1645 = CARTESIAN_POINT ( 'NONE',  ( 25.00000000000000355, 445.0000000000000568, -31.99999999999998579 ) ) ;
#1646 = CARTESIAN_POINT ( 'NONE',  ( 76.56941542346943663, 44.74353005244127246, 21.58911091692504769 ) ) ;
#1647 = ORIENTED_EDGE ( 'NONE', *, *, #9120, .F. ) ;
#1648 = CARTESIAN_POINT ( 'NONE',  ( 25.00000000000000000, 345.0000000000000568, -24.99999999999998934 ) ) ;
#1649 = CARTESIAN_POINT ( 'NONE',  ( -109.9268209223825750, 275.0000000000000000, 32.26598893414599445 ) ) ;
#1650 = CARTESIAN_POINT ( 'NONE',  ( -25.00000000000000000, 450.0000000000000568, -14.99999999999999289 ) ) ;
#1651 = VECTOR ( 'NONE', #598, 1000.000000000000000 ) ;
#1652 = CARTESIAN_POINT ( 'NONE',  ( -1.121994411437820194, 111.2499999986344079, -2.708734124999999437 ) ) ;
#1653 = ORIENTED_EDGE ( 'NONE', *, *, #8115, .F. ) ;
#1654 = CIRCLE ( 'NONE', #10398, 14.99999999999999822 ) ;
#1655 = EDGE_CURVE ( 'NONE', #8730, #5158, #12108, .T. ) ;
#1656 = CARTESIAN_POINT ( 'NONE',  ( 165.0000000000011369, 230.0000000000000853, -25.00000000000000000 ) ) ;
#1657 = EDGE_CURVE ( 'NONE', #3216, #11487, #625, .T. ) ;
#1658 = DIRECTION ( 'NONE',  ( 0.000000000000000000, 0.000000000000000000, 1.000000000000000000 ) ) ;
#1659 = CARTESIAN_POINT ( 'NONE',  ( -34.45294269781049223, 77.00000000000002842, 8.660253777987195534 ) ) ;
#1660 = DIRECTION ( 'NONE',  ( -0.000000000000000000, -0.000000000000000000, 1.000000000000000000 ) ) ;
#1661 = CARTESIAN_POINT ( 'NONE',  ( -28.82113438504157799, 85.77482169909444565, -9.367611059671812512 ) ) ;
#1662 = LINE ( 'NONE', #9559, #1529 ) ;
#1663 = CARTESIAN_POINT ( 'NONE',  ( 1.285879139104720633E-15, 165.5000000000000000, 10.49999999999999822 ) ) ;
#1664 = CARTESIAN_POINT ( 'NONE',  ( 1.346194077712559833, 112.8124999999999858, -3.250000000000000000 ) ) ;
#1665 = VECTOR ( 'NONE', #6592, 1000.000000000000000 ) ;
#1666 = DIRECTION ( 'NONE',  ( -0.7071067811865511255, -0.7071067811865440200, -0.000000000000000000 ) ) ;
#1667 = ADVANCED_FACE ( 'NONE', ( #3848 ), #10176, .T. ) ;
#1668 = DIRECTION ( 'NONE',  ( 0.000000000000000000, 0.000000000000000000, -1.000000000000000000 ) ) ;
#1669 = VERTEX_POINT ( 'NONE', #3557 ) ;
#1670 = CARTESIAN_POINT ( 'NONE',  ( -25.00000000000000000, 445.0000000000000568, -59.99999999999999289 ) ) ;
#1671 = STYLED_ITEM ( 'NONE', ( #11321 ), #763 ) ;
#1672 = AXIS2_PLACEMENT_3D ( 'NONE', #10853, #2316, #5437 ) ;
#1673 = EDGE_CURVE ( 'NONE', #10742, #4428, #2219, .T. ) ;
#1674 = FACE_OUTER_BOUND ( 'NONE', #6355, .T. ) ;
#1675 = CARTESIAN_POINT ( 'NONE',  ( -69.85388127645428824, 75.26794919243114634, 7.660254037844465458 ) ) ;
#1676 = EDGE_LOOP ( 'NONE', ( #6465, #3810, #10461, #7615 ) ) ;
#1677 = DIRECTION ( 'NONE',  ( -0.000000000000000000, -1.000000000000000000, -0.000000000000000000 ) ) ;
#1678 = DIRECTION ( 'NONE',  ( 1.000000000000000000, 0.000000000000000000, 0.000000000000000000 ) ) ;
#1679 = EDGE_LOOP ( 'NONE', ( #3569, #5275 ) ) ;
#1680 = FACE_OUTER_BOUND ( 'NONE', #11150, .T. ) ;
#1681 = ADVANCED_FACE ( 'NONE', ( #3971 ), #8284, .F. ) ;
#1682 = AXIS2_PLACEMENT_3D ( 'NONE', #1142, #6873, #1200 ) ;
#1683 = AXIS2_PLACEMENT_3D ( 'NONE', #10392, #1855, #932 ) ;
#1684 = ORIENTED_EDGE ( 'NONE', *, *, #1333, .F. ) ;
#1685 = CARTESIAN_POINT ( 'NONE',  ( 31.18707241436460365, 75.10640101998821194, -7.566984156997462740 ) ) ;
#1687 = ORIENTED_EDGE ( 'NONE', *, *, #11584, .F. ) ;
#1686 = DIRECTION ( 'NONE',  ( -0.000000000000000000, 1.000000000000000000, -0.000000000000000000 ) ) ;
#1688 = ORIENTED_EDGE ( 'NONE', *, *, #9305, .T. ) ;
#1689 = DIRECTION ( 'NONE',  ( 0.000000000000000000, 1.000000000000000000, 0.000000000000000000 ) ) ;
#1690 = CARTESIAN_POINT ( 'NONE',  ( -34.84179752789421514, 75.25738092153642356, 7.654152443798540872 ) ) ;
#1691 = ORIENTED_EDGE ( 'NONE', *, *, #12343, .F. ) ;
#1692 = SURFACE_STYLE_FILL_AREA ( #7487 ) ;
#1693 = AXIS2_PLACEMENT_3D ( 'NONE', #10136, #8329, #3602 ) ;
#1694 = DIRECTION ( 'NONE',  ( 0.000000000000000000, 0.000000000000000000, 1.000000000000000000 ) ) ;
#1695 =( BOUNDED_CURVE ( )  B_SPLINE_CURVE ( 2, ( #2630, #1701, #889, #7437, #8474 ),
 .UNSPECIFIED., .F., .F. ) 
 B_SPLINE_CURVE_WITH_KNOTS ( ( 3, 2, 3 ),
 ( 0.9375000000000007772, 0.9687500000000004441, 1.000000000000000000 ),
 .UNSPECIFIED. ) 
 CURVE ( )  GEOMETRIC_REPRESENTATION_ITEM ( )  RATIONAL_B_SPLINE_CURVE ( ( 0.9999999999999981126, 0.9238795325112886259, 1.000000000000000000, 0.9238795325112867385, 1.000000000000000000 ) ) 
 REPRESENTATION_ITEM ( '' )  );
#1696 = AXIS2_PLACEMENT_3D ( 'NONE', #11366, #10355, #4686 ) ;
#1697 = CARTESIAN_POINT ( 'NONE',  ( 2.500000000000000000, 1.178949249685212974, -2.042000000000001148 ) ) ;
#1698 = DIRECTION ( 'NONE',  ( 0.000000000000000000, 0.000000000000000000, 1.000000000000000000 ) ) ;
#1699 = ORIENTED_EDGE ( 'NONE', *, *, #1288, .T. ) ;
#1700 = CARTESIAN_POINT ( 'NONE',  ( -1.121994411437818862, 112.8749999986344079, 2.708734124999999882 ) ) ;
#1701 = CARTESIAN_POINT ( 'NONE',  ( 1.346194077712585591, 113.8125000000000142, -3.249999999999974687 ) ) ;
#1702 = VECTOR ( 'NONE', #8940, 1000.000000000000000 ) ;
#1703 = VECTOR ( 'NONE', #10156, 1000.000000000000114 ) ;
#1704 = ORIENTED_EDGE ( 'NONE', *, *, #10723, .F. ) ;
#1705 = PLANE ( 'NONE',  #7184 ) ;
#1706 = CARTESIAN_POINT ( 'NONE',  ( 70.40913241174638415, 46.55333156353304958, 25.83788073351891512 ) ) ;
#1707 = ORIENTED_EDGE ( 'NONE', *, *, #3947, .T. ) ;
#1708 = CARTESIAN_POINT ( 'NONE',  ( 20.55500000000001748, 0.000000000000000000, 2.500000000000000888 ) ) ;
#1709 = CARTESIAN_POINT ( 'NONE',  ( 72.29800075079560884, 49.93741478214614204, 19.95946618966863895 ) ) ;
#1710 = ORIENTED_EDGE ( 'NONE', *, *, #12207, .T. ) ;
#1711 = ADVANCED_FACE ( 'NONE', ( #11229 ), #8633, .T. ) ;
#1712 = DIRECTION ( 'NONE',  ( 0.000000000000000000, 0.000000000000000000, -1.000000000000000000 ) ) ;
#1713 = DIRECTION ( 'NONE',  ( 0.000000000000000000, -0.000000000000000000, 1.000000000000000000 ) ) ;
#1714 = CIRCLE ( 'NONE', #4900, 70.00000000000000000 ) ;
#1715 = CARTESIAN_POINT ( 'NONE',  ( -2.708734124999999882, 113.0624999986344079, 3.317242575922456639E-16 ) ) ;
#1716 = ADVANCED_FACE ( 'NONE', ( #986 ), #6775, .F. ) ;
#1717 = EDGE_LOOP ( 'NONE', ( #4444, #3307, #11764, #9702 ) ) ;
#1718 = SURFACE_STYLE_USAGE ( .BOTH. , #10116 ) ;
#1719 = AXIS2_PLACEMENT_3D ( 'NONE', #8085, #1554, #2298 ) ;
#1720 = CIRCLE ( 'NONE', #8675, 5.000000000000000000 ) ;
#1721 = CARTESIAN_POINT ( 'NONE',  ( 10.19254911989230727, 36.28349364905406560, 80.00000000000000000 ) ) ;
#1722 = CYLINDRICAL_SURFACE ( 'NONE', #1568, 3.250000000000000444 ) ;
#1723 = CARTESIAN_POINT ( 'NONE',  ( -30.55702146375036676, 77.00000000000001421, 5.949569453687718834 ) ) ;
#1724 = DIRECTION ( 'NONE',  ( 0.000000000000000000, 0.000000000000000000, 1.000000000000000000 ) ) ;
#1725 = CIRCLE ( 'NONE', #9672, 9.999999999999994671 ) ;
#1726 = CARTESIAN_POINT ( 'NONE',  ( -1.190781129305651387, 17.00000000000009237, 80.00000000000000000 ) ) ;
#1727 = CARTESIAN_POINT ( 'NONE',  ( -3.103867246957984438, 44.90412228795011629, 74.94096782355340736 ) ) ;
#1728 = CYLINDRICAL_SURFACE ( 'NONE', #642, 15.00000000000000000 ) ;
#1729 = ORIENTED_EDGE ( 'NONE', *, *, #2791, .T. ) ;
#1730 = CARTESIAN_POINT ( 'NONE',  ( -3.250000000000001776, 111.5624999999999858, -1.346194077712558723 ) ) ;
#1731 = CARTESIAN_POINT ( 'NONE',  ( -20.00000000000000355, 54.99999999999999289, 57.08203932499370836 ) ) ;
#1732 = AXIS2_PLACEMENT_3D ( 'NONE', #4755, #7623, #8611 ) ;
#1733 = CARTESIAN_POINT ( 'NONE',  ( 1.990051048614449116E-16, 113.1249999972688158, 3.250000000000000444 ) ) ;
#1734 = VERTEX_POINT ( 'NONE', #758 ) ;
#1735 = CARTESIAN_POINT ( 'NONE',  ( -119.9399947101603772, 285.0000000000000568, 35.20508015793608081 ) ) ;
#1736 = DIRECTION ( 'NONE',  ( 0.000000000000000000, 0.000000000000000000, 1.000000000000000000 ) ) ;
#1737 = FACE_OUTER_BOUND ( 'NONE', #11293, .T. ) ;
#1738 = ORIENTED_EDGE ( 'NONE', *, *, #11532, .F. ) ;
#1739 = FACE_BOUND ( 'NONE', #6832, .T. ) ;
#1740 = DIRECTION ( 'NONE',  ( 1.000000000000000000, 0.000000000000000000, 0.000000000000000000 ) ) ;
#1741 = ADVANCED_FACE ( 'NONE', ( #7427 ), #8571, .F. ) ;
#1742 = ORIENTED_EDGE ( 'NONE', *, *, #2513, .T. ) ;
#1743 = DIRECTION ( 'NONE',  ( 0.000000000000000000, 0.000000000000000000, 1.000000000000000000 ) ) ;
#1744 = VERTEX_POINT ( 'NONE', #8698 ) ;
#1745 = CARTESIAN_POINT ( 'NONE',  ( 31.06657576416735012, 76.26187158480907158, -8.234095398640720376 ) ) ;
#1746 = CARTESIAN_POINT ( 'NONE',  ( 30.43816488677641630, 83.71535165408627677, 2.971076217724753832 ) ) ;
#1747 = VERTEX_POINT ( 'NONE', #7649 ) ;
#1748 = DIRECTION ( 'NONE',  ( 1.000000000000000000, 0.000000000000000000, 0.000000000000000000 ) ) ;
#1749 = ORIENTED_EDGE ( 'NONE', *, *, #3284, .F. ) ;
#1750 = EDGE_CURVE ( 'NONE', #1040, #11448, #2977, .T. ) ;
#1751 = EDGE_CURVE ( 'NONE', #2693, #6100, #5845, .T. ) ;
#1752 = DIRECTION ( 'NONE',  ( 1.000000000000000000, 0.000000000000000000, 0.000000000000000000 ) ) ;
#1753 = LINE ( 'NONE', #1633, #4857 ) ;
#1754 = LINE ( 'NONE', #5438, #2930 ) ;
#1755 = CARTESIAN_POINT ( 'NONE',  ( -82.90657655639077461, 275.0000000000000000, 79.06642500897154946 ) ) ;
#1756 = CIRCLE ( 'NONE', #10100, 10.49999999999999822 ) ;
#1757 = ORIENTED_EDGE ( 'NONE', *, *, #5843, .F. ) ;
#1758 = CARTESIAN_POINT ( 'NONE',  ( 1.658621287961228320E-16, 113.8124999986344079, 2.708734124999999882 ) ) ;
#1759 = CARTESIAN_POINT ( 'NONE',  ( -7.474274778359196070, 18.61666975080236597, 80.00000000000000000 ) ) ;
#1760 = EDGE_CURVE ( 'NONE', #5507, #8953, #9981, .T. ) ;
#1761 = ORIENTED_EDGE ( 'NONE', *, *, #7465, .F. ) ;
#1762 = DIRECTION ( 'NONE',  ( -1.000000000000000000, 3.469446951953611033E-15, 0.000000000000000000 ) ) ;
#1763 = CARTESIAN_POINT ( 'NONE',  ( 71.22405252493085470, 48.64415124599927509, 23.50371070993386269 ) ) ;
#1764 = ORIENTED_EDGE ( 'NONE', *, *, #124, .F. ) ;
#1765 = CARTESIAN_POINT ( 'NONE',  ( 32.14616437604218646, 85.84037417286381810, 9.329764321300741514 ) ) ;
#1766 = CARTESIAN_POINT ( 'NONE',  ( 72.61843774138908714, 50.00000000000009237, 18.75000000000001421 ) ) ;
#1767 = ORIENTED_EDGE ( 'NONE', *, *, #8553, .F. ) ;
#1768 = CARTESIAN_POINT ( 'NONE',  ( 2.500000000000000000, 1.178949249685212974, -2.042000000000001148 ) ) ;
#1769 = CARTESIAN_POINT ( 'NONE',  ( 20.00000000000000355, 54.99999999999999289, -57.08203932499370836 ) ) ;
#1770 = CARTESIAN_POINT ( 'NONE',  ( 1.658621287961228320E-16, 111.8124999986344079, 2.708734124999999882 ) ) ;
#1771 = CARTESIAN_POINT ( 'NONE',  ( -1.121994411437820194, 111.2499999986344079, -2.708734124999999437 ) ) ;
#1772 = ORIENTED_EDGE ( 'NONE', *, *, #6771, .T. ) ;
#1773 = EDGE_CURVE ( 'NONE', #6428, #10397, #5217, .T. ) ;
#1774 = ADVANCED_FACE ( 'NONE', ( #1412 ), #7886, .T. ) ;
#1775 = CARTESIAN_POINT ( 'NONE',  ( -7.906085446029426755, 18.86875173514728488, 80.00000000000000000 ) ) ;
#1776 = CARTESIAN_POINT ( 'NONE',  ( 0.000000000000000000, 110.0000000000000000, 0.000000000000000000 ) ) ;
#1777 = ORIENTED_EDGE ( 'NONE', *, *, #8505, .T. ) ;
#1779 = EDGE_CURVE ( 'NONE', #301, #3643, #469, .T. ) ;
#1778 = CARTESIAN_POINT ( 'NONE',  ( -30.83210227225915290, 77.00000000000000000, 6.426308247889123137 ) ) ;
#1780 = VECTOR ( 'NONE', #2713, 1000.000000000000000 ) ;
#1781 = CARTESIAN_POINT ( 'NONE',  ( 0.000000000000000000, 52.00000000000000711, 0.000000000000000000 ) ) ;
#1782 = DIRECTION ( 'NONE',  ( 0.000000000000000000, 0.000000000000000000, 1.000000000000000000 ) ) ;
#1783 = LINE ( 'NONE', #9186, #2910 ) ;
#1784 = CARTESIAN_POINT ( 'NONE',  ( 0.000000000000000000, 264.9990000000000236, -59.99999999999999289 ) ) ;
#1785 = CARTESIAN_POINT ( 'NONE',  ( -25.00000000000000000, 445.0000000000000568, -59.99999999999999289 ) ) ;
#1786 = CIRCLE ( 'NONE', #8147, 12.99999999999999822 ) ;
#1787 = CARTESIAN_POINT ( 'NONE',  ( 8.125438539539757699, 18.23465150910980626, 74.55949004007592862 ) ) ;
#1788 = LINE ( 'NONE', #2723, #909 ) ;
#1789 = ORIENTED_EDGE ( 'NONE', *, *, #7766, .F. ) ;
#1790 = DIRECTION ( 'NONE',  ( 0.000000000000000000, 0.000000000000000000, 1.000000000000000000 ) ) ;
#1791 = FACE_OUTER_BOUND ( 'NONE', #528, .T. ) ;
#1792 = DIRECTION ( 'NONE',  ( 0.000000000000000000, 0.000000000000000000, -1.000000000000000000 ) ) ;
#1793 = VERTEX_POINT ( 'NONE', #8756 ) ;
#1794 = AXIS2_PLACEMENT_3D ( 'NONE', #6754, #11627, #4951 ) ;
#1795 = DIRECTION ( 'NONE',  ( 0.000000000000000000, 0.000000000000000000, 1.000000000000000000 ) ) ;
#1796 = CARTESIAN_POINT ( 'NONE',  ( -0.9407811293052825707, 17.00000000000008882, 80.00000000000000000 ) ) ;
#1797 = ORIENTED_EDGE ( 'NONE', *, *, #1926, .F. ) ;
#1798 = DIRECTION ( 'NONE',  ( 0.000000000000000000, 1.000000000000000000, 0.000000000000000000 ) ) ;
#1799 = B_SPLINE_CURVE_WITH_KNOTS ( 'NONE', 3,
 ( #9122, #535, #10819, #471, #4398, #9817, #7147, #7089, #3412, #11832, #10944, #1415, #12015, #8193 ),
 .UNSPECIFIED., .F., .F.,
 ( 4, 2, 2, 2, 2, 2, 4 ),
 ( 0.001978049138782353184, 0.002761379211137155940, 0.003544709283491958261, 0.004328039355846760583, 0.005111369428201563772, 0.006678029572911168416, 0.008244689717620771324 ),
 .UNSPECIFIED. ) ;
#1800 = CIRCLE ( 'NONE', #4387, 98.00000000000001421 ) ;
#1801 = CIRCLE ( 'NONE', #11565, 9.999999999999994671 ) ;
#1802 = TOROIDAL_SURFACE ( 'NONE', #2175, 25.00000000000000000, 10.00000000000000000 ) ;
#1803 = ORIENTED_EDGE ( 'NONE', *, *, #4104, .F. ) ;
#1804 = EDGE_CURVE ( 'NONE', #2631, #5525, #7982, .T. ) ;
#1805 = CARTESIAN_POINT ( 'NONE',  ( -31.74999999999995737, 0.000000000000000000, 0.000000000000000000 ) ) ;
#1806 = LINE ( 'NONE', #11225, #8415 ) ;
#1807 = EDGE_LOOP ( 'NONE', ( #2058, #5789, #5095, #6562 ) ) ;
#1808 = ADVANCED_FACE ( 'NONE', ( #2163 ), #10942, .T. ) ;
#1809 = PLANE ( 'NONE',  #727 ) ;
#1810 = EDGE_LOOP ( 'NONE', ( #105, #3051, #1136, #6544 ) ) ;
#1811 = DIRECTION ( 'NONE',  ( -1.000000000000000000, -0.000000000000000000, -0.000000000000000000 ) ) ;
#1813 = CARTESIAN_POINT ( 'NONE',  ( 3.250000000000000444, 110.0000000000000000, 0.000000000000000000 ) ) ;
#1812 = AXIS2_PLACEMENT_3D ( 'NONE', #4187, #3447, #1449 ) ;
#1814 = VECTOR ( 'NONE', #6503, 1000.000000000000000 ) ;
#1815 = CARTESIAN_POINT ( 'NONE',  ( 140.0000000000011369, 30.00000000000008882, -19.99999999999999645 ) ) ;
#1816 = EDGE_LOOP ( 'NONE', ( #6729, #7569, #2705, #7619 ) ) ;
#1817 = CARTESIAN_POINT ( 'NONE',  ( -4.975863863883684959E-16, 112.3124999986344079, -2.708734124999999882 ) ) ;
#1818 = DIRECTION ( 'NONE',  ( -0.000000000000000000, 1.000000000000000000, -0.000000000000000000 ) ) ;
#1819 = VECTOR ( 'NONE', #2010, 1000.000000000000000 ) ;
#1820 = VECTOR ( 'NONE', #8913, 1000.000000000000000 ) ;
#1821 = ORIENTED_EDGE ( 'NONE', *, *, #2734, .T. ) ;
#1822 = EDGE_CURVE ( 'NONE', #9024, #5307, #10195, .T. ) ;
#1823 = CARTESIAN_POINT ( 'NONE',  ( -1.190781129305651387, 17.00000000000009237, 80.00000000000000000 ) ) ;
#1824 = CARTESIAN_POINT ( 'NONE',  ( 70.96538090731311854, 48.09020517423687124, 24.26905913879962640 ) ) ;
#1825 = ORIENTED_EDGE ( 'NONE', *, *, #7480, .T. ) ;
#1826 = CARTESIAN_POINT ( 'NONE',  ( 3.250000000000000444, 110.0624999999999858, 1.346194077712559167 ) ) ;
#1827 = CYLINDRICAL_SURFACE ( 'NONE', #311, 10.49999999999999822 ) ;
#1828 = ORIENTED_EDGE ( 'NONE', *, *, #2846, .F. ) ;
#1829 = LINE ( 'NONE', #5639, #7508 ) ;
#1830 = FACE_OUTER_BOUND ( 'NONE', #7383, .T. ) ;
#1831 = AXIS2_PLACEMENT_3D ( 'NONE', #10884, #3158, #9815 ) ;
#1832 = CARTESIAN_POINT ( 'NONE',  ( 1.915364268218909150, 110.6874999986344079, 1.915364268218909150 ) ) ;
#1833 = DIRECTION ( 'NONE',  ( -0.000000000000000000, -0.000000000000000000, 1.000000000000000000 ) ) ;
#1834 = VERTEX_POINT ( 'NONE', #6029 ) ;
#1835 = ADVANCED_FACE ( 'NONE', ( #2283 ), #9754, .F. ) ;
#1836 = EDGE_CURVE ( 'NONE', #10799, #1569, #9879, .T. ) ;
#1837 = CARTESIAN_POINT ( 'NONE',  ( 0.000000000000000000, 92.00000000000000000, -25.50000000000000000 ) ) ;
#1838 = AXIS2_PLACEMENT_3D ( 'NONE', #3085, #6891, #522 ) ;
#1839 = ORIENTED_EDGE ( 'NONE', *, *, #9686, .T. ) ;
#1840 = DIRECTION ( 'NONE',  ( -1.000000000000000000, 0.000000000000000000, 0.000000000000000000 ) ) ;
#1841 = CARTESIAN_POINT ( 'NONE',  ( 0.000000000000000000, 265.0000000000000000, 0.000000000000000000 ) ) ;
#1842 = FACE_OUTER_BOUND ( 'NONE', #10044, .T. ) ;
#1843 = DIRECTION ( 'NONE',  ( 0.000000000000000000, 1.000000000000000000, 0.000000000000000000 ) ) ;
#1844 = CARTESIAN_POINT ( 'NONE',  ( 0.000000000000000000, 340.0000000000000000, 0.000000000000000000 ) ) ;
#1845 = EDGE_CURVE ( 'NONE', #1793, #9034, #5023, .T. ) ;
#1846 = CIRCLE ( 'NONE', #6229, 75.00000000000001421 ) ;
#1847 = CARTESIAN_POINT ( 'NONE',  ( 70.29663099721912545, 46.18241670634586171, -26.14423569115638912 ) ) ;
#1848 = DIRECTION ( 'NONE',  ( -0.000000000000000000, -1.000000000000000000, -0.000000000000000000 ) ) ;
#1849 = ORIENTED_EDGE ( 'NONE', *, *, #8354, .T. ) ;
#1850 = DIRECTION ( 'NONE',  ( -1.000000000000000000, 0.000000000000000000, 0.000000000000000000 ) ) ;
#1851 = CARTESIAN_POINT ( 'NONE',  ( 0.000000000000000000, 285.0000000000000568, 105.0000000000000426 ) ) ;
#1852 = CARTESIAN_POINT ( 'NONE',  ( 5.200000000000002842, 0.000000000000000000, 0.000000000000000000 ) ) ;
#1853 = ORIENTED_EDGE ( 'NONE', *, *, #9348, .T. ) ;
#1854 = AXIS2_PLACEMENT_3D ( 'NONE', #4718, #10633, #4846 ) ;
#1855 = DIRECTION ( 'NONE',  ( -0.000000000000000000, -1.000000000000000000, -0.000000000000000000 ) ) ;
#1856 = ADVANCED_FACE ( 'NONE', ( #6960 ), #11895, .F. ) ;
#1857 = CARTESIAN_POINT ( 'NONE',  ( 0.000000000000000000, 110.0000000000000000, 0.000000000000000000 ) ) ;
#1858 = ORIENTED_EDGE ( 'NONE', *, *, #1499, .T. ) ;
#1859 = CARTESIAN_POINT ( 'NONE',  ( -25.00000000000000000, 445.0000000000000568, -59.99999999999999289 ) ) ;
#1860 = CIRCLE ( 'NONE', #3464, 5.000000000000004441 ) ;
#1861 = EDGE_LOOP ( 'NONE', ( #5108, #9215, #11311, #11794 ) ) ;
#1862 = LINE ( 'NONE', #8522, #4334 ) ;
#1863 = CARTESIAN_POINT ( 'NONE',  ( 9.942549119892413856, 23.28349364905404428, 80.00000000000000000 ) ) ;
#1864 = EDGE_LOOP ( 'NONE', ( #10104, #8786, #1366, #11017 ) ) ;
#1865 = CARTESIAN_POINT ( 'NONE',  ( 33.37417589188917333, 76.99999999999998579, -8.451338748825380165 ) ) ;
#1866 = DIRECTION ( 'NONE',  ( 1.000000000000000000, 0.000000000000000000, 0.000000000000000000 ) ) ;
#1867 = ORIENTED_EDGE ( 'NONE', *, *, #7605, .F. ) ;
#1868 = CARTESIAN_POINT ( 'NONE',  ( 120.0000000000009948, 45.00000000000008527, 20.00000000000000000 ) ) ;
#1869 = CYLINDRICAL_SURFACE ( 'NONE', #4026, 9.999999999999994671 ) ;
#1870 = FACE_OUTER_BOUND ( 'NONE', #9953, .T. ) ;
#1871 = ADVANCED_FACE ( 'NONE', ( #5222 ), #8005, .T. ) ;
#1872 = VECTOR ( 'NONE', #9243, 1000.000000000000000 ) ;
#1873 = ORIENTED_EDGE ( 'NONE', *, *, #897, .F. ) ;
#1874 = CARTESIAN_POINT ( 'NONE',  ( 1.915364268218908705, 114.4374999986344079, -1.915364268218909594 ) ) ;
#1875 = CIRCLE ( 'NONE', #11248, 30.00000000000000355 ) ;
#1876 = CARTESIAN_POINT ( 'NONE',  ( -2.298097038856279806, 111.4999999972688158, -2.298097038856279362 ) ) ;
#1877 = EDGE_CURVE ( 'NONE', #11984, #12107, #2341, .T. ) ;
#1878 = ORIENTED_EDGE ( 'NONE', *, *, #10963, .T. ) ;
#1879 = FACE_BOUND ( 'NONE', #2862, .T. ) ;
#1880 = CARTESIAN_POINT ( 'NONE',  ( 69.52686081652184669, 40.00000000000009237, 28.12499999999999645 ) ) ;
#1881 = ORIENTED_EDGE ( 'NONE', *, *, #6930, .T. ) ;
#1882 = VECTOR ( 'NONE', #957, 1000.000000000000000 ) ;
#1883 = CARTESIAN_POINT ( 'NONE',  ( -5.970153145843347347E-16, 112.7500000000000000, -3.250000000000000444 ) ) ;
#1884 = CARTESIAN_POINT ( 'NONE',  ( 0.000000000000000000, 265.0000000000000000, 0.000000000000000000 ) ) ;
#1885 = EDGE_LOOP ( 'NONE', ( #8424, #7096, #8090, #5651 ) ) ;
#1886 = EDGE_CURVE ( 'NONE', #2508, #11122, #427, .T. ) ;
#1887 = LINE ( 'NONE', #3013, #5916 ) ;
#1888 = DIRECTION ( 'NONE',  ( -1.000000000000000000, 0.000000000000000000, 0.000000000000000000 ) ) ;
#1889 = DIRECTION ( 'NONE',  ( -1.000000000000000000, 0.000000000000000000, 0.000000000000000000 ) ) ;
#1890 = VECTOR ( 'NONE', #2398, 1000.000000000000000 ) ;
#1891 = EDGE_CURVE ( 'NONE', #10740, #686, #5100, .T. ) ;
#1892 = EDGE_CURVE ( 'NONE', #10506, #10768, #7516, .T. ) ;
#1893 = DIRECTION ( 'NONE',  ( 0.000000000000000000, 0.000000000000000000, -1.000000000000000000 ) ) ;
#1894 = TOROIDAL_SURFACE ( 'NONE', #8255, 90.00000000000002842, 8.000000000000000000 ) ;
#1895 = EDGE_LOOP ( 'NONE', ( #3084, #6423, #581, #4488 ) ) ;
#1896 = AXIS2_PLACEMENT_3D ( 'NONE', #10342, #2625, #9283 ) ;
#1897 = EDGE_LOOP ( 'NONE', ( #10651, #7896, #3999, #10787, #1426, #9113, #4225, #8537, #9822 ) ) ;
#1898 = AXIS2_PLACEMENT_3D ( 'NONE', #860, #4654, #3720 ) ;
#1899 = PRODUCT ( 'Locking Bowl Cover with Feed Chute', 'Locking Bowl Cover with Feed Chute', '', ( #8716 ) ) ;
#1900 = SURFACE_STYLE_USAGE ( .BOTH. , #9368 ) ;
#1901 = CARTESIAN_POINT ( 'NONE',  ( 74.16198487095665826, 20.00000000000009237, -25.00000000000000000 ) ) ;
#1902 = VERTEX_POINT ( 'NONE', #7086 ) ;
#1903 = DIRECTION ( 'NONE',  ( 0.000000000000000000, 0.000000000000000000, 1.000000000000000000 ) ) ;
#1904 = DIRECTION ( 'NONE',  ( 0.000000000000000000, 1.000000000000000000, 0.000000000000000000 ) ) ;
#1905 = DIRECTION ( 'NONE',  ( 0.000000000000000000, 0.000000000000000000, 1.000000000000000000 ) ) ;
#1906 = CARTESIAN_POINT ( 'NONE',  ( 0.000000000000000000, 50.00000000000000000, 0.000000000000000000 ) ) ;
#1907 = EDGE_CURVE ( 'NONE', #301, #5980, #6149, .T. ) ;
#1908 = ORIENTED_EDGE ( 'NONE', *, *, #1345, .T. ) ;
#1909 = CIRCLE ( 'NONE', #8861, 10.00000000000000178 ) ;
#1910 =( NAMED_UNIT ( * ) SI_UNIT ( $, .STERADIAN. ) SOLID_ANGLE_UNIT ( ) );
#1911 = AXIS2_PLACEMENT_3D ( 'NONE', #10684, #11693, #3144 ) ;
#1912 = UNCERTAINTY_MEASURE_WITH_UNIT (LENGTH_MEASURE( 1.000000000000000082E-05 ), #3561, 'distance_accuracy_value', 'NONE');
#1913 = CARTESIAN_POINT ( 'NONE',  ( 75.64991689405155739, 43.99492456696821563, -23.01117105493013781 ) ) ;
#1914 = AXIS2_PLACEMENT_3D ( 'NONE', #4529, #10376, #4585 ) ;
#1915 = SURFACE_SIDE_STYLE ('',( #7709 ) ) ;
#1916 = ORIENTED_EDGE ( 'NONE', *, *, #9580, .F. ) ;
#1917 = LINE ( 'NONE', #7586, #3656 ) ;
#1918 = CARTESIAN_POINT ( 'NONE',  ( -69.85388127645428824, 77.76794919243110371, 3.330127018922237614 ) ) ;
#1919 = FACE_OUTER_BOUND ( 'NONE', #3235, .T. ) ;
#1920 = FACE_OUTER_BOUND ( 'NONE', #7935, .T. ) ;
#1921 = VERTEX_POINT ( 'NONE', #11007 ) ;
#1922 = LINE ( 'NONE', #4919, #4271 ) ;
#1923 = ORIENTED_EDGE ( 'NONE', *, *, #4088, .F. ) ;
#1924 = CARTESIAN_POINT ( 'NONE',  ( 4.025725221640669815, 38.53525403784453118, 80.00000000000000000 ) ) ;
#1925 = CIRCLE ( 'NONE', #5120, 65.00000000000001421 ) ;
#1926 = EDGE_CURVE ( 'NONE', #8236, #8588, #7273, .T. ) ;
#1927 = ORIENTED_EDGE ( 'NONE', *, *, #4103, .F. ) ;
#1928 = EDGE_CURVE ( 'NONE', #10032, #9030, #3589, .T. ) ;
#1929 = CARTESIAN_POINT ( 'NONE',  ( -12.57411137850303540, 36.28349364905398033, 79.50000000000000000 ) ) ;
#1930 = DIRECTION ( 'NONE',  ( -1.000000000000000000, -0.000000000000000000, -0.000000000000000000 ) ) ;
#1931 = ORIENTED_EDGE ( 'NONE', *, *, #2094, .F. ) ;
#1932 = AXIS2_PLACEMENT_3D ( 'NONE', #5152, #8871, #3211 ) ;
#1933 = CARTESIAN_POINT ( 'NONE',  ( -5.970153145843347347E-16, 111.6249999972688158, -3.250000000000000444 ) ) ;
#1934 = DIRECTION ( 'NONE',  ( -1.000000000000000000, -0.000000000000000000, -0.000000000000000000 ) ) ;
#1935 = ORIENTED_EDGE ( 'NONE', *, *, #9515, .T. ) ;
#1936 = EDGE_CURVE ( 'NONE', #5710, #7852, #2422, .T. ) ;
#1937 = APPLICATION_PROTOCOL_DEFINITION ( 'draft international standard', 'automotive_design', 1998, #3826 ) ;
#1938 = DIRECTION ( 'NONE',  ( -0.5000000000000051070, 1.060575238724903217E-16, -0.8660254037844355990 ) ) ;
#1939 = DIRECTION ( 'NONE',  ( 0.000000000000000000, -0.8660254037844407060, 0.4999999999999965028 ) ) ;
#1940 = DIRECTION ( 'NONE',  ( 1.000000000000000000, 0.000000000000000000, 0.000000000000000000 ) ) ;
#1941 = VERTEX_POINT ( 'NONE', #11134 ) ;
#1942 = CARTESIAN_POINT ( 'NONE',  ( 1.658621287961228320E-16, 112.8124999986344079, 2.708734124999999882 ) ) ;
#1943 = CARTESIAN_POINT ( 'NONE',  ( 1.346194077712559389, 111.0624999972688016, 3.250000000000000444 ) ) ;
#1944 = ORIENTED_EDGE ( 'NONE', *, *, #12194, .T. ) ;
#1945 = CARTESIAN_POINT ( 'NONE',  ( 140.0000000000011369, 67.07106781186550393, 20.00000000000000000 ) ) ;
#1946 = CARTESIAN_POINT ( 'NONE',  ( 20.00000000000000355, 50.00000000000000000, 57.08203932499370836 ) ) ;
#1947 = EDGE_LOOP ( 'NONE', ( #4493, #4209, #2967, #5069 ) ) ;
#1948 = CARTESIAN_POINT ( 'NONE',  ( 2.298097038856279806, 110.1250000000000000, 2.298097038856279806 ) ) ;
#1949 = CARTESIAN_POINT ( 'NONE',  ( 170.0000000000011369, 225.0000000000000853, 20.00000000000000000 ) ) ;
#1950 = ORIENTED_EDGE ( 'NONE', *, *, #7796, .F. ) ;
#1951 = CARTESIAN_POINT ( 'NONE',  ( 0.000000000000000000, 5.000000000000129674, 70.00000000000001421 ) ) ;
#1952 = CARTESIAN_POINT ( 'NONE',  ( 0.000000000000000000, 65.00000000000000000, 0.000000000000000000 ) ) ;
#1953 = CARTESIAN_POINT ( 'NONE',  ( -1.121994411437820194, 114.2499999986344079, -2.708734124999999437 ) ) ;
#1954 = CARTESIAN_POINT ( 'NONE',  ( 2.298097038856278918, 113.8750000000000000, -2.298097038856279806 ) ) ;
#1955 = DIRECTION ( 'NONE',  ( -0.000000000000000000, -1.000000000000000000, -0.000000000000000000 ) ) ;
#1956 = ORIENTED_EDGE ( 'NONE', *, *, #11945, .T. ) ;
#1957 = CIRCLE ( 'NONE', #2153, 15.00000000000000000 ) ;
#1958 = EDGE_CURVE ( 'NONE', #12281, #3955, #5339, .T. ) ;
#1959 = MECHANICAL_DESIGN_GEOMETRIC_PRESENTATION_REPRESENTATION (  '', ( #10160 ), #3359 ) ;
#1960 = VERTEX_POINT ( 'NONE', #11199 ) ;
#1961 = DIRECTION ( 'NONE',  ( -0.000000000000000000, -1.000000000000000000, -0.000000000000000000 ) ) ;
#1962 = CARTESIAN_POINT ( 'NONE',  ( 1.734723475976807094E-14, 63.00000000000000000, 57.08203932499370836 ) ) ;
#1963 = ORIENTED_EDGE ( 'NONE', *, *, #701, .F. ) ;
#1964 = EDGE_CURVE ( 'NONE', #5986, #7898, #10984, .T. ) ;
#1965 = DIRECTION ( 'NONE',  ( -0.4999999999999985012, -0.8660254037844394848, 0.000000000000000000 ) ) ;
#1966 = DIRECTION ( 'NONE',  ( 0.000000000000000000, 1.000000000000000000, 0.000000000000000000 ) ) ;
#1967 = CARTESIAN_POINT ( 'NONE',  ( 69.52686081652184669, 50.00000000000000000, 28.12500000000000000 ) ) ;
#1968 = CARTESIAN_POINT ( 'NONE',  ( 9.942549119892305498, 36.71650635094628967, 79.50000000000000000 ) ) ;
#1969 = PRODUCT_DEFINITION_FORMATION_WITH_SPECIFIED_SOURCE ( 'ANY', '', #11777, .NOT_KNOWN. ) ;
#1970 = ORIENTED_EDGE ( 'NONE', *, *, #4392, .F. ) ;
#1971 = CARTESIAN_POINT ( 'NONE',  ( 0.000000000000000000, 75.00000000000001421, 0.000000000000000000 ) ) ;
#1972 = EDGE_CURVE ( 'NONE', #8477, #5671, #3650, .T. ) ;
#1973 = ADVANCED_FACE ( 'NONE', ( #1597 ), #7398, .T. ) ;
#1974 = CARTESIAN_POINT ( 'NONE',  ( 70.67517779188629845, 47.36270866767235077, -25.10124566575549210 ) ) ;
#1975 = CARTESIAN_POINT ( 'NONE',  ( 5.092712519748611832, 18.61666975080242992, 79.50000000000000000 ) ) ;
#1976 = CARTESIAN_POINT ( 'NONE',  ( 0.000000000000000000, 75.00000000000000000, 0.000000000000000000 ) ) ;
#1977 = DIRECTION ( 'NONE',  ( 0.000000000000000000, 0.000000000000000000, 1.000000000000000000 ) ) ;
#1978 = CARTESIAN_POINT ( 'NONE',  ( 70.23094937779806912, 14.08906915838008089, -26.31821466697866185 ) ) ;
#1979 = ORIENTED_EDGE ( 'NONE', *, *, #215, .F. ) ;
#1980 = PLANE ( 'NONE',  #888 ) ;
#1981 = DIRECTION ( 'NONE',  ( 0.000000000000000000, 0.000000000000000000, 1.000000000000000000 ) ) ;
#1982 = CIRCLE ( 'NONE', #2777, 10.00000000000000178 ) ;
#1983 = VECTOR ( 'NONE', #835, 1000.000000000000000 ) ;
#1984 = ORIENTED_EDGE ( 'NONE', *, *, #9038, .T. ) ;
#1985 = STYLED_ITEM ( 'NONE', ( #11194 ), #4372 ) ;
#1986 = CARTESIAN_POINT ( 'NONE',  ( -25.00000000000000000, 445.0000000000000568, -29.99999999999999289 ) ) ;
#1987 = ADVANCED_FACE ( 'NONE', ( #9119 ), #11951, .T. ) ;
#1988 = ADVANCED_FACE ( 'NONE', ( #2650 ), #5616, .F. ) ;
#1989 = ORIENTED_EDGE ( 'NONE', *, *, #5014, .F. ) ;
#1990 = DIRECTION ( 'NONE',  ( -0.4999999999999942268, 0.8660254037844419273, 0.000000000000000000 ) ) ;
#1991 = CARTESIAN_POINT ( 'NONE',  ( 74.40419232661420779, 41.74530093123432550, 24.69784343973813634 ) ) ;
#1992 = ORIENTED_EDGE ( 'NONE', *, *, #448, .T. ) ;
#1993 = LINE ( 'NONE', #9706, #1494 ) ;
#1994 = PLANE ( 'NONE',  #4105 ) ;
#1995 = VERTEX_POINT ( 'NONE', #6273 ) ;
#1996 = ITEM_DEFINED_TRANSFORMATION ( 'NONE', 'NONE', #1371,  #1612 ) ;
#1997 = CARTESIAN_POINT ( 'NONE',  ( 0.000000000000000000, 65.00000000000000000, -70.00000000000001421 ) ) ;
#1998 = DIRECTION ( 'NONE',  ( -3.469446951953619119E-16, 0.000000000000000000, -1.000000000000000000 ) ) ;
#1999 = DIRECTION ( 'NONE',  ( 0.000000000000000000, 1.000000000000000000, 0.000000000000000000 ) ) ;
#2000 = ORIENTED_EDGE ( 'NONE', *, *, #11440, .T. ) ;
#2001 = CARTESIAN_POINT ( 'NONE',  ( -2.708734125000000326, 112.8124999986344079, 3.317242575922457132E-16 ) ) ;
#2002 = ADVANCED_FACE ( 'NONE', ( #3469 ), #11075, .F. ) ;
#2003 = CARTESIAN_POINT ( 'NONE',  ( 2.298097038856278918, 111.7499999972688158, -2.298097038856279806 ) ) ;
#2004 = AXIS2_PLACEMENT_3D ( 'NONE', #8641, #10522, #1180 ) ;
#2005 = AXIS2_PLACEMENT_3D ( 'NONE', #3086, #11696, #6893 ) ;
#2006 = EDGE_LOOP ( 'NONE', ( #1565, #9158 ) ) ;
#2007 = CARTESIAN_POINT ( 'NONE',  ( -89.80805993797480369, 285.0000000000000568, 81.82974571984181011 ) ) ;
#2008 = CARTESIAN_POINT ( 'NONE',  ( 0.000000000000000000, 50.00000000000000000, 0.000000000000000000 ) ) ;
#2009 = ORIENTED_EDGE ( 'NONE', *, *, #9960, .T. ) ;
#2010 = DIRECTION ( 'NONE',  ( -0.000000000000000000, -1.000000000000000000, -0.000000000000000000 ) ) ;
#2011 = DIRECTION ( 'NONE',  ( 0.000000000000000000, 0.000000000000000000, 1.000000000000000000 ) ) ;
#2012 = AXIS2_PLACEMENT_3D ( 'NONE', #1769, #2701, #3696 ) ;
#2013 = ORIENTED_EDGE ( 'NONE', *, *, #11200, .T. ) ;
#2014 = DIRECTION ( 'NONE',  ( 0.000000000000000000, -0.000000000000000000, 1.000000000000000000 ) ) ;
#2015 = CARTESIAN_POINT ( 'NONE',  ( -20.00000000000004263, 7.965803112215716020, 67.08203932499370126 ) ) ;
#2016 = LINE ( 'NONE', #7864, #10761 ) ;
#2017 = DIRECTION ( 'NONE',  ( 0.8660254037844420383, 0.4999999999999942824, 0.000000000000000000 ) ) ;
#2018 = CARTESIAN_POINT ( 'NONE',  ( 0.000000000000000000, 165.0000000000000000, 0.000000000000000000 ) ) ;
#2019 = EDGE_CURVE ( 'NONE', #5470, #8579, #11159, .T. ) ;
#2020 = AXIS2_PLACEMENT_3D ( 'NONE', #97, #11523, #34 ) ;
#2021 = CARTESIAN_POINT ( 'NONE',  ( 1.915364268218909150, 113.6874999986344079, 1.915364268218909150 ) ) ;
#2022 = ORIENTED_EDGE ( 'NONE', *, *, #8900, .F. ) ;
#2023 = PRESENTATION_STYLE_ASSIGNMENT (( #10618 ) ) ;
#2024 = TOROIDAL_SURFACE ( 'NONE', #8969, 110.0000000000000284, 5.000000000000000000 ) ;
#2025 = ORIENTED_EDGE ( 'NONE', *, *, #11728, .T. ) ;
#2026 = DIRECTION ( 'NONE',  ( -0.000000000000000000, 1.000000000000000000, -0.000000000000000000 ) ) ;
#2027 = CARTESIAN_POINT ( 'NONE',  ( 6.210137148270883145, 43.08033144994158903, 74.74717517330344663 ) ) ;
#2028 = ORIENTED_EDGE ( 'NONE', *, *, #7862, .F. ) ;
#2029 = AXIS2_PLACEMENT_3D ( 'NONE', #4331, #8256, #6334 ) ;
#2030 = PLANE ( 'NONE',  #7218 ) ;
#2031 = DIRECTION ( 'NONE',  ( 1.000000000000000000, -0.000000000000000000, 0.000000000000000000 ) ) ;
#2032 = CIRCLE ( 'NONE', #9579, 9.999999999999994671 ) ;
#2033 = CARTESIAN_POINT ( 'NONE',  ( -30.25776724459628753, 76.75431408359612817, 5.085794527760020500 ) ) ;
#2034 = CARTESIAN_POINT ( 'NONE',  ( -1.915364268218909816, 110.9374999986344079, -1.915364268218909150 ) ) ;
#2035 = VERTEX_POINT ( 'NONE', #6214 ) ;
#2036 = ADVANCED_FACE ( 'NONE', ( #8130 ), #5531, .F. ) ;
#2037 = ADVANCED_FACE ( 'NONE', ( #9184, #662 ), #8377, .T. ) ;
#2038 = EDGE_CURVE ( 'NONE', #2522, #434, #7207, .T. ) ;
#2039 = CARTESIAN_POINT ( 'NONE',  ( 71.00573438501002954, 48.18030900481924306, -24.15070487907424734 ) ) ;
#2040 = DIRECTION ( 'NONE',  ( 0.000000000000000000, 0.4999999999999962808, 0.8660254037844407060 ) ) ;
#2041 =( BOUNDED_SURFACE ( )  B_SPLINE_SURFACE ( 3, 2, ( 
 ( #422, #4344, #6287 ),
 ( #8948, #3423, #2353 ),
 ( #614, #3294, #7097 ),
 ( #9131, #3232, #6042 ) ),
 .UNSPECIFIED., .F., .F., .F. ) 
 B_SPLINE_SURFACE_WITH_KNOTS ( ( 4, 4 ),
 ( 3, 3 ),
 ( 0.08252307147638787699, 0.08572545668793386808 ),
 ( 0.000000000000000000, 1.000000000000000000 ),
 .UNSPECIFIED. ) 
 GEOMETRIC_REPRESENTATION_ITEM ( )  RATIONAL_B_SPLINE_SURFACE ( (
 ( 1.000000000000000000, 0.8237544710479146604, 1.000000000000000000),
 ( 1.000000000000000000, 0.8337078205039558654, 1.000000000000000000),
 ( 1.000000000000000000, 0.8426243553970736988, 1.000000000000000000),
 ( 1.000000000000000000, 0.8507194741069452615, 1.000000000000000000) ) ) 
 REPRESENTATION_ITEM ( '' )  SURFACE ( )  );
#2042 = DIRECTION ( 'NONE',  ( 0.7071067811865513475, 0.7071067811865437980, -0.000000000000000000 ) ) ;
#2043 = CARTESIAN_POINT ( 'NONE',  ( 72.61843774138908714, 10.00000000000009059, -18.74999999999999289 ) ) ;
#2044 = ORIENTED_EDGE ( 'NONE', *, *, #4713, .T. ) ;
#2045 = DIRECTION ( 'NONE',  ( -0.4999999999999942268, 0.8660254037844419273, 0.000000000000000000 ) ) ;
#2046 = CARTESIAN_POINT ( 'NONE',  ( -11.19078112930532498, 30.25000000000005684, 79.50000000000000000 ) ) ;
#2047 = AXIS2_PLACEMENT_3D ( 'NONE', #976, #1096, #84 ) ;
#2048 = EDGE_LOOP ( 'NONE', ( #7070, #1054, #7481, #6311 ) ) ;
#2049 = DIRECTION ( 'NONE',  ( 0.000000000000000000, 0.000000000000000000, -1.000000000000000000 ) ) ;
#2050 = EDGE_CURVE ( 'NONE', #6378, #11448, #6157, .T. ) ;
#2051 = ORIENTED_EDGE ( 'NONE', *, *, #4623, .F. ) ;
#2052 = AXIS2_PLACEMENT_3D ( 'NONE', #2556, #3243, #9968 ) ;
#2053 = DIRECTION ( 'NONE',  ( -0.8660254037844394848, -0.4999999999999985567, 0.000000000000000000 ) ) ;
#2054 = CARTESIAN_POINT ( 'NONE',  ( 0.000000000000000000, 260.0000000000000000, 105.0000000000000426 ) ) ;
#2055 = ORIENTED_EDGE ( 'NONE', *, *, #2920, .F. ) ;
#2056 = DIRECTION ( 'NONE',  ( 0.000000000000000000, 1.000000000000000000, 0.000000000000000000 ) ) ;
#2057 = FACE_OUTER_BOUND ( 'NONE', #5797, .T. ) ;
#2058 = ORIENTED_EDGE ( 'NONE', *, *, #5528, .T. ) ;
#2059 = APPLICATION_PROTOCOL_DEFINITION ( 'draft international standard', 'automotive_design', 1998, #4862 ) ;
#2060 = DIRECTION ( 'NONE',  ( 0.000000000000000000, 1.000000000000000000, 0.000000000000000000 ) ) ;
#2061 = CARTESIAN_POINT ( 'NONE',  ( 0.000000000000000000, 87.00000000000000000, 0.000000000000000000 ) ) ;
#2062 = EDGE_CURVE ( 'NONE', #4939, #2386, #791, .T. ) ;
#2063 = ADVANCED_FACE ( 'NONE', ( #3962 ), #8562, .T. ) ;
#2064 = VERTEX_POINT ( 'NONE', #9558 ) ;
#2065 = VECTOR ( 'NONE', #5965, 1000.000000000000114 ) ;
#2066 = CARTESIAN_POINT ( 'NONE',  ( 1.346194077712559833, 112.6874999972688158, -3.250000000000000000 ) ) ;
#2067 = ORIENTED_EDGE ( 'NONE', *, *, #3141, .F. ) ;
#2068 = PLANE ( 'NONE',  #8935 ) ;
#2069 = SPHERICAL_SURFACE ( 'NONE', #9040, 5.000000000000000000 ) ;
#2070 = EDGE_LOOP ( 'NONE', ( #3023, #6435, #6345, #7354 ) ) ;
#2071 = CYLINDRICAL_SURFACE ( 'NONE', #7788, 9.999999999999994671 ) ;
#2072 = FACE_OUTER_BOUND ( 'NONE', #6725, .T. ) ;
#2073 = ORIENTED_EDGE ( 'NONE', *, *, #8808, .F. ) ;
#2074 = VECTOR ( 'NONE', #3021, 1000.000000000000000 ) ;
#2075 = VECTOR ( 'NONE', #3237, 1000.000000000000000 ) ;
#2076 = FACE_OUTER_BOUND ( 'NONE', #10289, .T. ) ;
#2077 = DIRECTION ( 'NONE',  ( -0.5000000000000006661, -0.8660254037844383745, 0.000000000000000000 ) ) ;
#2078 = DIRECTION ( 'NONE',  ( -3.469446951953613203E-16, 0.000000000000000000, -1.000000000000000000 ) ) ;
#2079 = CARTESIAN_POINT ( 'NONE',  ( 1.121994411437819084, 114.3749999986344221, -2.708734124999999437 ) ) ;
#2080 = CARTESIAN_POINT ( 'NONE',  ( -7.546443561989872428, 41.34166358254155682, 80.00000048127353125 ) ) ;
#2081 = CARTESIAN_POINT ( 'NONE',  ( 2.708734124999999437, 114.4999999986344079, -1.121994411437820416 ) ) ;
#2082 =( NAMED_UNIT ( * ) PLANE_ANGLE_UNIT ( ) SI_UNIT ( $, .RADIAN. ) );
#2083 = AXIS2_PLACEMENT_3D ( 'NONE', #3919, #8638, #990 ) ;
#2084 = VERTEX_POINT ( 'NONE', #4705 ) ;
#2085 = EDGE_CURVE ( 'NONE', #4062, #4534, #5791, .T. ) ;
#2086 = CARTESIAN_POINT ( 'NONE',  ( 117.9289321881355193, 45.00000000000008527, 25.00000000000000000 ) ) ;
#2087 = EDGE_CURVE ( 'NONE', #11761, #6384, #7576, .T. ) ;
#2088 = CARTESIAN_POINT ( 'NONE',  ( 2.500000000000000000, -1.178949249685218748, -2.041999999999998039 ) ) ;
#2089 = EDGE_LOOP ( 'NONE', ( #9140, #4210, #268, #10094 ) ) ;
#2090 = DIRECTION ( 'NONE',  ( 0.000000000000000000, -0.000000000000000000, 1.000000000000000000 ) ) ;
#2091 = CARTESIAN_POINT ( 'NONE',  ( -89.80805993797480369, 275.0000000000000000, 71.82974571984181011 ) ) ;
#2092 = DIRECTION ( 'NONE',  ( 0.000000000000000000, 1.000000000000000000, 0.000000000000000000 ) ) ;
#2093 = CARTESIAN_POINT ( 'NONE',  ( -2.708734125000000326, 110.7499999986343937, 1.121994411437819084 ) ) ;
#2094 = EDGE_CURVE ( 'NONE', #7950, #6913, #1190, .T. ) ;
#2095 = VECTOR ( 'NONE', #1614, 1000.000000000000000 ) ;
#2096 = ORIENTED_EDGE ( 'NONE', *, *, #11598, .F. ) ;
#2097 =( BOUNDED_CURVE ( )  B_SPLINE_CURVE ( 2, ( #8481, #11182, #3753, #2636, #2697, #6444, #6509, #10235, #1883 ),
 .UNSPECIFIED., .F., .F. ) 
 B_SPLINE_CURVE_WITH_KNOTS ( ( 3, 2, 2, 2, 3 ),
 ( 0.5625000000000004441, 0.5937500000000004441, 0.6250000000000004441, 0.6562500000000005551, 0.6875000000000005551 ),
 .UNSPECIFIED. ) 
 CURVE ( )  GEOMETRIC_REPRESENTATION_ITEM ( )  RATIONAL_B_SPLINE_CURVE ( ( 0.9999999999999988898, 0.9238795325112878487, 1.000000000000000000, 0.9238795325112867385, 1.000000000000000000, 0.9238795325112867385, 1.000000000000000000, 0.9238795325112854062, 1.000000000000001332 ) ) 
 REPRESENTATION_ITEM ( '' )  );
#2098 = AXIS2_PLACEMENT_3D ( 'NONE', #2517, #5324, #1579 ) ;
#2099 = VERTEX_POINT ( 'NONE', #9372 ) ;
#2100 =( NAMED_UNIT ( * ) SI_UNIT ( $, .STERADIAN. ) SOLID_ANGLE_UNIT ( ) );
#2101 = ORIENTED_EDGE ( 'NONE', *, *, #3184, .T. ) ;
#2102 = VECTOR ( 'NONE', #7528, 1000.000000000000000 ) ;
#2103 = FILL_AREA_STYLE ('',( #3219 ) ) ;
#2104 = DIRECTION ( 'NONE',  ( 0.000000000000000000, 1.000000000000000000, 0.000000000000000000 ) ) ;
#2105 = DIRECTION ( 'NONE',  ( 0.000000000000000000, -0.8660254037844402619, -0.4999999999999975575 ) ) ;
#2106 = CARTESIAN_POINT ( 'NONE',  ( -12.32411137850302119, 23.28349364905396612, 80.00000000000000000 ) ) ;
#2107 = CARTESIAN_POINT ( 'NONE',  ( 70.52159520668648440, 13.08551330184377370, -25.52954545350316451 ) ) ;
#2108 = ORIENTED_EDGE ( 'NONE', *, *, #7108, .F. ) ;
#2109 = CARTESIAN_POINT ( 'NONE',  ( 1.990051048614449116E-16, 111.2500000000000000, 3.250000000000000444 ) ) ;
#2110 = PRODUCT_DEFINITION_SHAPE ( 'NONE', 'NONE',  #4743 ) ;
#2111 = CARTESIAN_POINT ( 'NONE',  ( 11.80921887069452580, 30.00000000000008882, 78.00000000000000000 ) ) ;
#2112 = AXIS2_PLACEMENT_3D ( 'NONE', #7503, #649, #5637 ) ;
#2113 = VERTEX_POINT ( 'NONE', #3709 ) ;
#2114 = CARTESIAN_POINT ( 'NONE',  ( -34.73110591274434000, 77.00000000000000000, 8.660254037844445918 ) ) ;
#2115 = AXIS2_PLACEMENT_3D ( 'NONE', #745, #1615, #6476 ) ;
#2116 = ORIENTED_EDGE ( 'NONE', *, *, #4989, .F. ) ;
#2117 = FACE_OUTER_BOUND ( 'NONE', #209, .T. ) ;
#2118 = DIRECTION ( 'NONE',  ( -0.000000000000000000, -0.000000000000000000, 1.000000000000000000 ) ) ;
#2119 = VERTEX_POINT ( 'NONE', #5837 ) ;
#2120 = CARTESIAN_POINT ( 'NONE',  ( -1.190781129305471087, 30.00000000000008882, 80.00000000000000000 ) ) ;
#2121 = DIRECTION ( 'NONE',  ( -1.000000000000000000, 0.000000000000000000, 0.000000000000000000 ) ) ;
#2122 = ORIENTED_EDGE ( 'NONE', *, *, #2843, .F. ) ;
#2123 = EDGE_CURVE ( 'NONE', #10790, #5372, #4591, .T. ) ;
#2124 = CARTESIAN_POINT ( 'NONE',  ( -9.726035167149728267, 35.21650635094616888, 80.00000000000000000 ) ) ;
#2125 = FACE_BOUND ( 'NONE', #709, .T. ) ;
#2126 = ORIENTED_EDGE ( 'NONE', *, *, #277, .T. ) ;
#2127 = CARTESIAN_POINT ( 'NONE',  ( -1.915364268218909816, 111.9374999986344079, -1.915364268218909150 ) ) ;
#2128 = CARTESIAN_POINT ( 'NONE',  ( -1.346194077712559389, 113.1874999972688016, 3.250000000000000444 ) ) ;
#2129 = CIRCLE ( 'NONE', #9484, 125.0000000000000284 ) ;
#2130 = ORIENTED_EDGE ( 'NONE', *, *, #1964, .T. ) ;
#2131 = EDGE_CURVE ( 'NONE', #10138, #2113, #915, .T. ) ;
#2132 = CARTESIAN_POINT ( 'NONE',  ( 9.942549119892305498, 36.71650635094628967, 80.00000000000000000 ) ) ;
#2133 = CARTESIAN_POINT ( 'NONE',  ( -13.10975425465743172, 20.87853446539744340, 73.84596017914877564 ) ) ;
#2134 = VERTEX_POINT ( 'NONE', #6706 ) ;
#2135 = CARTESIAN_POINT ( 'NONE',  ( 2.500000000000000000, 1.178949249685217415, 2.041999999999998483 ) ) ;
#2136 = LINE ( 'NONE', #3129, #6292 ) ;
#2137 = ORIENTED_EDGE ( 'NONE', *, *, #3757, .F. ) ;
#2138 = CARTESIAN_POINT ( 'NONE',  ( 1.408343819019456413E-14, 285.0000000000000568, 115.0000000000000284 ) ) ;
#2139 = DIRECTION ( 'NONE',  ( -0.000000000000000000, 1.000000000000000000, -0.000000000000000000 ) ) ;
#2140 = LINE ( 'NONE', #1024, #5199 ) ;
#2141 = CARTESIAN_POINT ( 'NONE',  ( 0.000000000000000000, 153.0000000000000000, 0.000000000000000000 ) ) ;
#2142 = LINE ( 'NONE', #2197, #2388 ) ;
#2143 = CARTESIAN_POINT ( 'NONE',  ( 2.708734124999999437, 112.4999999986343937, -1.121994411437820416 ) ) ;
#2144 = ORIENTED_EDGE ( 'NONE', *, *, #8075, .T. ) ;
#2145 = ORIENTED_EDGE ( 'NONE', *, *, #510, .T. ) ;
#2146 = CARTESIAN_POINT ( 'NONE',  ( 0.000000000000000000, 265.0000000000000000, 100.0000000000000284 ) ) ;
#2147 = FACE_OUTER_BOUND ( 'NONE', #2962, .T. ) ;
#2148 = ORIENTED_EDGE ( 'NONE', *, *, #2426, .F. ) ;
#2149 = CARTESIAN_POINT ( 'NONE',  ( 150.0000000000010800, 15.00000000000008882, 25.00000000000000000 ) ) ;
#2150 = DIRECTION ( 'NONE',  ( 0.000000000000000000, 0.000000000000000000, 1.000000000000000000 ) ) ;
#2151 = CARTESIAN_POINT ( 'NONE',  ( -12.44911137850304250, 36.50000000000007816, 80.00000000000000000 ) ) ;
#2152 = DIRECTION ( 'NONE',  ( 0.000000000000000000, 0.000000000000000000, -1.000000000000000000 ) ) ;
#2153 = AXIS2_PLACEMENT_3D ( 'NONE', #9084, #6545, #5305 ) ;
#2154 = ORIENTED_EDGE ( 'NONE', *, *, #8061, .T. ) ;
#2155 =( NAMED_UNIT ( * ) PLANE_ANGLE_UNIT ( ) SI_UNIT ( $, .RADIAN. ) );
#2156 = EDGE_CURVE ( 'NONE', #7734, #4551, #8738, .T. ) ;
#2157 = ORIENTED_EDGE ( 'NONE', *, *, #2279, .F. ) ;
#2158 = EDGE_CURVE ( 'NONE', #1095, #5322, #3373, .T. ) ;
#2159 = CARTESIAN_POINT ( 'NONE',  ( -6.000000000000000000, 62.00000000000000000, 70.00000000000001421 ) ) ;
#2160 = AXIS2_PLACEMENT_3D ( 'NONE', #8559, #9307, #9427 ) ;
#2161 = DIRECTION ( 'NONE',  ( 0.000000000000000000, 0.000000000000000000, 1.000000000000000000 ) ) ;
#2162 =( GEOMETRIC_REPRESENTATION_CONTEXT ( 3 ) GLOBAL_UNCERTAINTY_ASSIGNED_CONTEXT ( ( #7522 ) ) GLOBAL_UNIT_ASSIGNED_CONTEXT ( ( #5830, #2082, #3956 ) ) REPRESENTATION_CONTEXT ( 'NONE', 'WORKASPACE' ) );
#2163 = FACE_OUTER_BOUND ( 'NONE', #8054, .T. ) ;
#2164 = DIRECTION ( 'NONE',  ( -0.000000000000000000, -0.000000000000000000, 1.000000000000000000 ) ) ;
#2165 = CARTESIAN_POINT ( 'NONE',  ( 72.18749001408211541, 14.85617579097899288, -20.39424303846762498 ) ) ;
#2166 = DIRECTION ( 'NONE',  ( 0.000000000000000000, 1.000000000000000000, 0.000000000000000000 ) ) ;
#2167 = DIRECTION ( 'NONE',  ( 1.000000000000000000, 0.000000000000000000, 0.000000000000000000 ) ) ;
#2168 = ORIENTED_EDGE ( 'NONE', *, *, #1456, .T. ) ;
#2169 = CARTESIAN_POINT ( 'NONE',  ( 0.000000000000000000, 275.0000000000000000, 0.000000000000000000 ) ) ;
#2170 = EDGE_LOOP ( 'NONE', ( #1120, #3244, #10555, #5195 ) ) ;
#2171 = DIRECTION ( 'NONE',  ( 3.469446951953613203E-16, 0.000000000000000000, -1.000000000000000000 ) ) ;
#2172 = EDGE_LOOP ( 'NONE', ( #1385, #4057, #975, #1609, #12259 ) ) ;
#2173 = ORIENTED_EDGE ( 'NONE', *, *, #3226, .F. ) ;
#2174 = CIRCLE ( 'NONE', #9126, 12.99999999999999822 ) ;
#2175 = AXIS2_PLACEMENT_3D ( 'NONE', #10101, #6379, #710 ) ;
#2176 = CARTESIAN_POINT ( 'NONE',  ( 0.000000000000000000, 225.0000000000000853, -20.00000000000000000 ) ) ;
#2177 = CARTESIAN_POINT ( 'NONE',  ( 9.184850993605151889E-15, 50.00000000000000000, 75.00000000000002842 ) ) ;
#2178 = ORIENTED_EDGE ( 'NONE', *, *, #2305, .T. ) ;
#2179 = CARTESIAN_POINT ( 'NONE',  ( -1.121994411437818862, 111.6249999986344079, 2.708734125000000326 ) ) ;
#2180 = CARTESIAN_POINT ( 'NONE',  ( 1.990051048614449116E-16, 114.1249999972688158, 3.250000000000000444 ) ) ;
#2181 = EDGE_CURVE ( 'NONE', #3552, #3229, #1097, .T. ) ;
#2182 = AXIS2_PLACEMENT_3D ( 'NONE', #2553, #6356, #1496 ) ;
#2183 = EDGE_CURVE ( 'NONE', #7236, #5974, #11966, .T. ) ;
#2184 = ORIENTED_EDGE ( 'NONE', *, *, #10586, .T. ) ;
#2185 = AXIS2_PLACEMENT_3D ( 'NONE', #11626, #6879, #10677 ) ;
#2186 = CARTESIAN_POINT ( 'NONE',  ( 0.000000000000000000, 92.00000000000000000, 0.000000000000000000 ) ) ;
#2187 = CARTESIAN_POINT ( 'NONE',  ( -16.19078112930547064, 30.00000000000008882, 65.00000000000000000 ) ) ;
#2188 = ORIENTED_EDGE ( 'NONE', *, *, #1595, .T. ) ;
#2189 = AXIS2_PLACEMENT_3D ( 'NONE', #11175, #10227, #123 ) ;
#2190 = CARTESIAN_POINT ( 'NONE',  ( 25.00000000000000000, 450.0000000000000568, -14.99999999999998934 ) ) ;
#2191 = CARTESIAN_POINT ( 'NONE',  ( 71.66825662749600667, 10.65753464538973994, 22.10769995529666332 ) ) ;
#2192 = EDGE_LOOP ( 'NONE', ( #7675, #746, #11330, #2503 ) ) ;
#2193 = LINE ( 'NONE', #3012, #9052 ) ;
#2194 = CARTESIAN_POINT ( 'NONE',  ( 74.75803814165917061, 42.66597992467871592, -24.24257051231691307 ) ) ;
#2195 = FACE_OUTER_BOUND ( 'NONE', #5983, .T. ) ;
#2196 = ORIENTED_EDGE ( 'NONE', *, *, #2512, .F. ) ;
#2197 = CARTESIAN_POINT ( 'NONE',  ( -25.00000000000000000, 445.0000000000000568, -24.99999999999998934 ) ) ;
#2198 = CARTESIAN_POINT ( 'NONE',  ( 2.708734124999999882, 111.6249999986343937, 1.121994411437819084 ) ) ;
#2199 = EDGE_CURVE ( 'NONE', #6075, #10794, #11387, .T. ) ;
#2200 = TOROIDAL_SURFACE ( 'NONE', #2603, 9.999999999999998224, 5.000000000000000000 ) ;
#2201 = ORIENTED_EDGE ( 'NONE', *, *, #3226, .T. ) ;
#2202 = CARTESIAN_POINT ( 'NONE',  ( 76.77549258727734127, 15.14783244007807994, 21.24643021050508551 ) ) ;
#2203 = AXIS2_PLACEMENT_3D ( 'NONE', #3595, #5413, #2656 ) ;
#2204 = EDGE_LOOP ( 'NONE', ( #3819, #880, #11119, #3936, #1212 ) ) ;
#2205 = PRODUCT_DEFINITION_SHAPE ( 'NONE', 'NONE',  #12360 ) ;
#2206 = LINE ( 'NONE', #11633, #2074 ) ;
#2207 = LINE ( 'NONE', #6016, #11478 ) ;
#2208 = ORIENTED_EDGE ( 'NONE', *, *, #2759, .T. ) ;
#2209 = CARTESIAN_POINT ( 'NONE',  ( 0.000000000000000000, 115.0000000000000000, -9.999999999999998224 ) ) ;
#2210 = CARTESIAN_POINT ( 'NONE',  ( 0.000000000000000000, 67.00000000000000000, 25.00000000000000000 ) ) ;
#2211 = DIRECTION ( 'NONE',  ( 0.000000000000000000, 0.000000000000000000, -1.000000000000000000 ) ) ;
#2212 = CARTESIAN_POINT ( 'NONE',  ( 145.0000000000011369, 0.000000000000000000, -25.00000000000000000 ) ) ;
#2213 = AXIS2_PLACEMENT_3D ( 'NONE', #1131, #55, #10532 ) ;
#2214 = ADVANCED_FACE ( 'NONE', ( #8625 ), #4646, .T. ) ;
#2215 = EDGE_CURVE ( 'NONE', #9788, #5829, #977, .T. ) ;
#2216 = ORIENTED_EDGE ( 'NONE', *, *, #6232, .F. ) ;
#2217 = SURFACE_STYLE_USAGE ( .BOTH. , #1347 ) ;
#2218 = ORIENTED_EDGE ( 'NONE', *, *, #5864, .T. ) ;
#2219 = CIRCLE ( 'NONE', #3217, 4.999999999999998224 ) ;
#2220 = SURFACE_SIDE_STYLE ('',( #11703 ) ) ;
#2221 = AXIS2_PLACEMENT_3D ( 'NONE', #4678, #8469, #12295 ) ;
#2222 = DIRECTION ( 'NONE',  ( -1.000000000000000000, 0.000000000000000000, 0.000000000000000000 ) ) ;
#2223 = CARTESIAN_POINT ( 'NONE',  ( -27.33018067101282256, 87.00000000000000000, -12.37179148263487605 ) ) ;
#2224 = DIRECTION ( 'NONE',  ( -1.000000000000000000, 0.000000000000000000, 0.000000000000000000 ) ) ;
#2225 = CARTESIAN_POINT ( 'NONE',  ( 9.942549119892413856, 23.28349364905404428, 80.00000000000000000 ) ) ;
#2226 = CARTESIAN_POINT ( 'NONE',  ( -9.976035167149682081, 25.21650635094616533, 79.50000000000000000 ) ) ;
#2227 = CARTESIAN_POINT ( 'NONE',  ( -4.975863863883684959E-16, 113.0624999986344079, -2.708734125000000326 ) ) ;
#2228 = ORIENTED_EDGE ( 'NONE', *, *, #8855, .T. ) ;
#2229 = CARTESIAN_POINT ( 'NONE',  ( 0.000000000000000000, 165.5000000000000000, 0.000000000000000000 ) ) ;
#2230 = ORIENTED_EDGE ( 'NONE', *, *, #8427, .F. ) ;
#2231 = ORIENTED_EDGE ( 'NONE', *, *, #6662, .T. ) ;
#2232 = FACE_OUTER_BOUND ( 'NONE', #9916, .T. ) ;
#2233 = EDGE_CURVE ( 'NONE', #7634, #1834, #7698, .T. ) ;
#2234 = DIRECTION ( 'NONE',  ( 0.000000000000000000, 0.000000000000000000, 1.000000000000000000 ) ) ;
#2235 = ORIENTED_EDGE ( 'NONE', *, *, #10451, .T. ) ;
#2236 = VECTOR ( 'NONE', #9557, 1000.000000000000000 ) ;
#2237 = CARTESIAN_POINT ( 'NONE',  ( -24.99999999999999645, 450.0000000000000568, -105.0000000000000000 ) ) ;
#2238 = CARTESIAN_POINT ( 'NONE',  ( 8.939921633775681592E-15, 65.00000000000000000, 73.00000000000002842 ) ) ;
#2239 = EDGE_CURVE ( 'NONE', #11257, #4695, #6763, .T. ) ;
#2240 = ORIENTED_EDGE ( 'NONE', *, *, #3782, .F. ) ;
#2241 = CARTESIAN_POINT ( 'NONE',  ( -2.708734125000000770, 110.8749999986343937, -1.121994411437818639 ) ) ;
#2242 = AXIS2_PLACEMENT_3D ( 'NONE', #12105, #11601, #8711 ) ;
#2243 = VERTEX_POINT ( 'NONE', #6526 ) ;
#2244 = DIRECTION ( 'NONE',  ( 0.000000000000000000, 0.000000000000000000, 1.000000000000000000 ) ) ;
#2245 = DIRECTION ( 'NONE',  ( 0.000000000000000000, 0.000000000000000000, -1.000000000000000000 ) ) ;
#2246 = VERTEX_POINT ( 'NONE', #10311 ) ;
#2247 = FACE_OUTER_BOUND ( 'NONE', #12228, .T. ) ;
#2248 = DIRECTION ( 'NONE',  ( -0.000000000000000000, 1.000000000000000000, -0.000000000000000000 ) ) ;
#2249 = EDGE_CURVE ( 'NONE', #5904, #9892, #8139, .T. ) ;
#2250 = ORIENTED_EDGE ( 'NONE', *, *, #4793, .T. ) ;
#2251 = CARTESIAN_POINT ( 'NONE',  ( 2.500000000000000000, 2.357898499370431722, -2.818925648462311528E-15 ) ) ;
#2252 = CARTESIAN_POINT ( 'NONE',  ( -6.407287480251391720, 21.46474596215567487, 80.00000000000000000 ) ) ;
#2253 = DIRECTION ( 'NONE',  ( -1.000000000000000000, -0.000000000000000000, -0.000000000000000000 ) ) ;
#2254 = VECTOR ( 'NONE', #7647, 1000.000000000000000 ) ;
#2255 = ORIENTED_EDGE ( 'NONE', *, *, #4879, .F. ) ;
#2256 = LINE ( 'NONE', #137, #5973 ) ;
#2257 = ADVANCED_FACE ( 'NONE', ( #10374 ), #2772, .T. ) ;
#2258 = CARTESIAN_POINT ( 'NONE',  ( 69.52686081653675387, 19.66584645497869843, 28.12499999996316546 ) ) ;
#2259 = VERTEX_POINT ( 'NONE', #4961 ) ;
#2260 = CARTESIAN_POINT ( 'NONE',  ( 1.990051048614449116E-16, 112.1249999972688158, 3.250000000000000444 ) ) ;
#2261 = CARTESIAN_POINT ( 'NONE',  ( 69.53320273752093783, 40.66811906995093295, -28.10933780299387763 ) ) ;
#2262 = AXIS2_PLACEMENT_3D ( 'NONE', #3647, #12199, #5711 ) ;
#2263 = AXIS2_PLACEMENT_3D ( 'NONE', #6307, #4185, #3445 ) ;
#2264 = VERTEX_POINT ( 'NONE', #7878 ) ;
#2265 = PRODUCT_DEFINITION_CONTEXT ( 'detailed design', #5510, 'design' ) ;
#2266 = CARTESIAN_POINT ( 'NONE',  ( 34.73110591274434000, 77.00000000000000000, -8.660254037844445918 ) ) ;
#2267 = CARTESIAN_POINT ( 'NONE',  ( 71.54748821555412519, 44.36552556075854881, 22.64388168110885857 ) ) ;
#2268 = EDGE_LOOP ( 'NONE', ( #10266, #8033, #7306, #7027, #11755, #11420, #6855, #438 ) ) ;
#2269 = DIRECTION ( 'NONE',  ( 0.000000000000000000, 0.000000000000000000, 1.000000000000000000 ) ) ;
#2270 = DIRECTION ( 'NONE',  ( -0.000000000000000000, -1.000000000000000000, -0.000000000000000000 ) ) ;
#2271 = CARTESIAN_POINT ( 'NONE',  ( 0.000000000000000000, 110.0000000000000000, 0.000000000000000000 ) ) ;
#2272 = CARTESIAN_POINT ( 'NONE',  ( -23.51709844389219839, 11.48290155610792063, -57.08203932499370836 ) ) ;
#2273 = EDGE_CURVE ( 'NONE', #7990, #2035, #1401, .T. ) ;
#2274 = VERTEX_POINT ( 'NONE', #6139 ) ;
#2275 = AXIS2_PLACEMENT_3D ( 'NONE', #8359, #2881, #4752 ) ;
#2276 = SHAPE_REPRESENTATION_RELATIONSHIP ( 'NONE' , 'NONE' ,  #7136, #7202 ) ;
#2277 = CIRCLE ( 'NONE', #1285, 25.50000000000000000 ) ;
#2278 = ORIENTED_EDGE ( 'NONE', *, *, #9929, .T. ) ;
#2279 = EDGE_CURVE ( 'NONE', #3932, #7967, #5569, .T. ) ;
#2280 = EDGE_CURVE ( 'NONE', #2560, #5411, #8990, .T. ) ;
#2281 = DIRECTION ( 'NONE',  ( 0.000000000000000000, 0.8660254037844405950, -0.4999999999999965028 ) ) ;
#2282 = AXIS2_PLACEMENT_3D ( 'NONE', #2664, #6475, #5356 ) ;
#2283 = FACE_OUTER_BOUND ( 'NONE', #10867, .T. ) ;
#2284 = CIRCLE ( 'NONE', #697, 9.999999999999998224 ) ;
#2285 =( LENGTH_UNIT ( ) NAMED_UNIT ( * ) SI_UNIT ( .MILLI., .METRE. ) );
#2286 = DIRECTION ( 'NONE',  ( -0.7236679289129753778, 0.000000000000000000, 0.6901483381584025967 ) ) ;
#2287 = CARTESIAN_POINT ( 'NONE',  ( -116.4243635975518742, 275.0000000000000000, 45.50129185973785440 ) ) ;
#2288 = CARTESIAN_POINT ( 'NONE',  ( -3.250000000000000444, 110.4375000000000000, 1.346194077712559389 ) ) ;
#2289 = ORIENTED_EDGE ( 'NONE', *, *, #10112, .T. ) ;
#2290 = DIRECTION ( 'NONE',  ( 0.000000000000000000, 0.000000000000000000, -1.000000000000000000 ) ) ;
#2291 = EDGE_CURVE ( 'NONE', #12245, #5612, #7386, .T. ) ;
#2292 = VECTOR ( 'NONE', #1172, 1000.000000000000000 ) ;
#2293 = CIRCLE ( 'NONE', #69, 90.00000000000002842 ) ;
#2294 = ORIENTED_EDGE ( 'NONE', *, *, #4258, .T. ) ;
#2295 = FACE_OUTER_BOUND ( 'NONE', #3987, .T. ) ;
#2296 = ORIENTED_EDGE ( 'NONE', *, *, #7572, .T. ) ;
#2297 = CARTESIAN_POINT ( 'NONE',  ( 34.84121487603211875, 75.26794919243111792, -7.660254037844449471 ) ) ;
#2298 = DIRECTION ( 'NONE',  ( 0.000000000000000000, 0.000000000000000000, 1.000000000000000000 ) ) ;
#2299 = ORIENTED_EDGE ( 'NONE', *, *, #3925, .T. ) ;
#2300 = VECTOR ( 'NONE', #10486, 1000.000000000000114 ) ;
#2301 = CARTESIAN_POINT ( 'NONE',  ( -25.00000000000000000, 445.0000000000000568, -59.99999999999999289 ) ) ;
#2302 = ORIENTED_EDGE ( 'NONE', *, *, #7763, .F. ) ;
#2303 = CARTESIAN_POINT ( 'NONE',  ( 70.07436679451828354, 45.25447089753193808, -26.73229126030999581 ) ) ;
#2304 = TOROIDAL_SURFACE ( 'NONE', #2708, 24.99999999999999645, 0.5000000000000004441 ) ;
#2305 = EDGE_CURVE ( 'NONE', #4827, #12106, #9680, .T. ) ;
#2306 = ADVANCED_FACE ( 'NONE', ( #1220 ), #6079, .F. ) ;
#2307 = AXIS2_PLACEMENT_3D ( 'NONE', #3679, #1748, #7365 ) ;
#2308 = ORIENTED_EDGE ( 'NONE', *, *, #6327, .T. ) ;
#2309 = CARTESIAN_POINT ( 'NONE',  ( 32.15778161310143446, 87.00000000000000000, 8.660254037844435260 ) ) ;
#2310 = EDGE_CURVE ( 'NONE', #2754, #4316, #4490, .T. ) ;
#2311 = VERTEX_POINT ( 'NONE', #5898 ) ;
#2312 = CONICAL_SURFACE ( 'NONE', #12283, 2.041999999999999815, 1.047197551196591858 ) ;
#2313 = DIRECTION ( 'NONE',  ( 1.000000000000000000, 0.000000000000000000, 0.000000000000000000 ) ) ;
#2314 = FACE_BOUND ( 'NONE', #10934, .T. ) ;
#2315 = ORIENTED_EDGE ( 'NONE', *, *, #4354, .F. ) ;
#2316 = DIRECTION ( 'NONE',  ( 0.000000000000000000, 1.000000000000000000, 0.000000000000000000 ) ) ;
#2317 = CARTESIAN_POINT ( 'NONE',  ( 75.04559065614574820, 43.19565876339696331, -23.85935468423092587 ) ) ;
#2318 = CARTESIAN_POINT ( 'NONE',  ( 5.309218870694559556, 41.25833024919784719, 80.00000000000000000 ) ) ;
#2319 = ORIENTED_EDGE ( 'NONE', *, *, #8930, .F. ) ;
#2320 = CARTESIAN_POINT ( 'NONE',  ( 3.061616997868382648E-15, 87.00000000000000000, -24.99999999999999645 ) ) ;
#2321 = CARTESIAN_POINT ( 'NONE',  ( 69.87020289360386016, 15.79423913611491948, 27.26117375607985593 ) ) ;
#2322 = VECTOR ( 'NONE', #2139, 1000.000000000000000 ) ;
#2323 = VERTEX_POINT ( 'NONE', #3265 ) ;
#2324 = CARTESIAN_POINT ( 'NONE',  ( 76.84533340411822167, 44.87486296789415974, -21.12320159127844832 ) ) ;
#2325 = CARTESIAN_POINT ( 'NONE',  ( -12.32411137850302119, 23.28349364905396612, 80.00000000000000000 ) ) ;
#2326 = ORIENTED_EDGE ( 'NONE', *, *, #4166, .F. ) ;
#2327 = CARTESIAN_POINT ( 'NONE',  ( 30.00100000000000122, 75.26794919243111792, 7.660254037844449471 ) ) ;
#2328 = CARTESIAN_POINT ( 'NONE',  ( 71.26470115309105324, 43.60909254972982296, 23.55923316143271151 ) ) ;
#2329 = VERTEX_POINT ( 'NONE', #11758 ) ;
#2330 = DIRECTION ( 'NONE',  ( 0.000000000000000000, 0.8660254037844407060, -0.4999999999999965583 ) ) ;
#2331 = LINE ( 'NONE', #7821, #9326 ) ;
#2332 = PRESENTATION_STYLE_ASSIGNMENT (( #5210 ) ) ;
#2333 = CARTESIAN_POINT ( 'NONE',  ( 2.708734125000000326, 112.3749999986344079, 1.121994411437819084 ) ) ;
#2334 = ADVANCED_FACE ( 'NONE', ( #4084, #1158 ), #4024, .F. ) ;
#2335 = ORIENTED_EDGE ( 'NONE', *, *, #1377, .T. ) ;
#2336 = ORIENTED_EDGE ( 'NONE', *, *, #7763, .T. ) ;
#2337 = EDGE_CURVE ( 'NONE', #1631, #9640, #2331, .T. ) ;
#2338 = FILL_AREA_STYLE_COLOUR ( '', #6280 ) ;
#2339 = CARTESIAN_POINT ( 'NONE',  ( -29.42287733398164207, 85.62135522733750292, -10.27237124600374685 ) ) ;
#2340 = CARTESIAN_POINT ( 'NONE',  ( 30.00000000000004263, 65.00000000000000000, -57.08203932499370836 ) ) ;
#2341 = LINE ( 'NONE', #4034, #842 ) ;
#2342 = PRESENTATION_STYLE_ASSIGNMENT (( #11772 ) ) ;
#2343 = LINE ( 'NONE', #9063, #3912 ) ;
#2344 = AXIS2_PLACEMENT_3D ( 'NONE', #4238, #3309, #1318 ) ;
#2345 = CARTESIAN_POINT ( 'NONE',  ( 72.28493664348422953, 10.06798366438096615, -20.00732221823095003 ) ) ;
#2346 = CARTESIAN_POINT ( 'NONE',  ( -1.915364268218909816, 110.9374999986344079, -1.915364268218909150 ) ) ;
#2347 = EDGE_LOOP ( 'NONE', ( #132, #1214 ) ) ;
#2348 = CARTESIAN_POINT ( 'NONE',  ( 1.285879139104721264E-14, 260.0000000000000000, -105.0000000000000426 ) ) ;
#2349 = EDGE_CURVE ( 'NONE', #6428, #1442, #9552, .T. ) ;
#2350 = CIRCLE ( 'NONE', #6943, 70.00000000000001421 ) ;
#2351 = EDGE_CURVE ( 'NONE', #7682, #7936, #6187, .T. ) ;
#2352 = ORIENTED_EDGE ( 'NONE', *, *, #6920, .F. ) ;
#2353 = CARTESIAN_POINT ( 'NONE',  ( 32.12519652190606223, 85.41823950547951938, 9.573483885149325801 ) ) ;
#2354 = VERTEX_POINT ( 'NONE', #5957 ) ;
#2355 = DIRECTION ( 'NONE',  ( 0.000000000000000000, 1.000000000000000000, 0.000000000000000000 ) ) ;
#2356 = CARTESIAN_POINT ( 'NONE',  ( 170.0000000000011369, 35.00000000000004974, 25.00000000000000000 ) ) ;
#2357 = ORIENTED_EDGE ( 'NONE', *, *, #9659, .F. ) ;
#2358 = DIRECTION ( 'NONE',  ( 0.000000000000000000, -0.000000000000000000, 1.000000000000000000 ) ) ;
#2359 = CARTESIAN_POINT ( 'NONE',  ( -1.440781129305471087, 40.00000000000008527, 79.50000000000000000 ) ) ;
#2360 = ORIENTED_EDGE ( 'NONE', *, *, #7154, .T. ) ;
#2361 = VERTEX_POINT ( 'NONE', #2210 ) ;
#2362 = CARTESIAN_POINT ( 'NONE',  ( 3.980102097228898231E-16, 110.0000000000000000, -3.250000000000000444 ) ) ;
#2363 = ADVANCED_FACE ( 'NONE', ( #1281 ), #9740, .F. ) ;
#2364 = ADVANCED_FACE ( 'NONE', ( #9805 ), #3210, .T. ) ;
#2365 = ORIENTED_EDGE ( 'NONE', *, *, #1877, .F. ) ;
#2366 = CARTESIAN_POINT ( 'NONE',  ( 29.32777202433393526, 87.43477800909943198, 9.413311639618298088 ) ) ;
#2367 = DIRECTION ( 'NONE',  ( 3.469446951953613203E-16, -0.000000000000000000, 1.000000000000000000 ) ) ;
#2368 = AXIS2_PLACEMENT_3D ( 'NONE', #8807, #274, #7012 ) ;
#2369 = ORIENTED_EDGE ( 'NONE', *, *, #2920, .T. ) ;
#2370 = CARTESIAN_POINT ( 'NONE',  ( -7.907287480251421030, 41.13333024919781167, 80.00000000000000000 ) ) ;
#2371 = LINE ( 'NONE', #8968, #9868 ) ;
#2372 = ORIENTED_EDGE ( 'NONE', *, *, #5795, .T. ) ;
#2373 = LINE ( 'NONE', #8911, #7667 ) ;
#2374 = DIRECTION ( 'NONE',  ( 0.000000000000000000, 0.000000000000000000, 1.000000000000000000 ) ) ;
#2375 = FACE_OUTER_BOUND ( 'NONE', #2172, .T. ) ;
#2376 = VERTEX_POINT ( 'NONE', #3333 ) ;
#2377 = CARTESIAN_POINT ( 'NONE',  ( 2.708734124999999882, 110.6249999986343937, 1.121994411437818862 ) ) ;
#2378 = CARTESIAN_POINT ( 'NONE',  ( 71.43334412524814070, 10.98941133951209892, 22.86096127246252863 ) ) ;
#2379 = AXIS2_PLACEMENT_3D ( 'NONE', #1857, #4662, #7293 ) ;
#2380 = ORIENTED_EDGE ( 'NONE', *, *, #7548, .T. ) ;
#2381 = CARTESIAN_POINT ( 'NONE',  ( 71.78384618016781360, 49.48703820365247452, -21.72949947218331701 ) ) ;
#2382 = FACE_OUTER_BOUND ( 'NONE', #8509, .T. ) ;
#2383 = ORIENTED_EDGE ( 'NONE', *, *, #7916, .F. ) ;
#2384 = DIRECTION ( 'NONE',  ( -1.000000000000000000, -0.000000000000000000, -0.000000000000000000 ) ) ;
#2385 = CARTESIAN_POINT ( 'NONE',  ( 70.79098555896973721, 40.43144037915666900, 24.99999999902148318 ) ) ;
#2386 = VERTEX_POINT ( 'NONE', #9992 ) ;
#2387 = DIRECTION ( 'NONE',  ( 0.000000000000000000, 0.000000000000000000, -1.000000000000000000 ) ) ;
#2388 = VECTOR ( 'NONE', #5945, 1000.000000000000000 ) ;
#2389 = FACE_OUTER_BOUND ( 'NONE', #3479, .T. ) ;
#2390 = ADVANCED_FACE ( 'NONE', ( #10930, #2389 ), #1464, .T. ) ;
#2391 = CARTESIAN_POINT ( 'NONE',  ( 0.000000000000000000, 260.0000000000000000, 0.000000000000000000 ) ) ;
#2392 = CARTESIAN_POINT ( 'NONE',  ( -1.121994411437820194, 112.9999999986344079, -2.708734124999999882 ) ) ;
#2393 = ORIENTED_EDGE ( 'NONE', *, *, #6090, .F. ) ;
#2394 = ORIENTED_EDGE ( 'NONE', *, *, #8117, .F. ) ;
#2395 = AXIS2_PLACEMENT_3D ( 'NONE', #8079, #11840, #8888 ) ;
#2396 = AXIS2_PLACEMENT_3D ( 'NONE', #8499, #10502, #12320 ) ;
#2397 = UNCERTAINTY_MEASURE_WITH_UNIT (LENGTH_MEASURE( 1.000000000000000082E-05 ), #218, 'distance_accuracy_value', 'NONE');
#2398 = DIRECTION ( 'NONE',  ( 0.000000000000000000, 0.000000000000000000, -1.000000000000000000 ) ) ;
#2399 = CYLINDRICAL_SURFACE ( 'NONE', #5552, 5.000000000000000000 ) ;
#2400 = DIRECTION ( 'NONE',  ( 3.469446951953613203E-16, 0.000000000000000000, 1.000000000000000000 ) ) ;
#2401 = CARTESIAN_POINT ( 'NONE',  ( -27.52813290908667909, 87.44182241851447657, -11.93450069589770202 ) ) ;
#2402 = CARTESIAN_POINT ( 'NONE',  ( -12.57411137850303540, 36.28349364905398033, 80.00000000000000000 ) ) ;
#2403 = VECTOR ( 'NONE', #7745, 1000.000000000000000 ) ;
#2404 = DIRECTION ( 'NONE',  ( 0.000000000000000000, 1.000000000000000000, 0.000000000000000000 ) ) ;
#2405 = AXIS2_PLACEMENT_3D ( 'NONE', #10012, #786, #2410 ) ;
#2406 = LINE ( 'NONE', #6338, #5017 ) ;
#2407 = CARTESIAN_POINT ( 'NONE',  ( 165.0000000000011369, 37.07106781186553945, 25.00000000000000000 ) ) ;
#2408 = CARTESIAN_POINT ( 'NONE',  ( -4.975863863883684959E-16, 111.0624999986344079, -2.708734125000000326 ) ) ;
#2409 = EDGE_CURVE ( 'NONE', #8944, #2376, #10932, .T. ) ;
#2410 = DIRECTION ( 'NONE',  ( -0.7236679289129653858, 0.000000000000000000, -0.6901483381584129218 ) ) ;
#2411 = FACE_OUTER_BOUND ( 'NONE', #5638, .T. ) ;
#2412 = ADVANCED_FACE ( 'NONE', ( #7499 ), #1705, .T. ) ;
#2413 = AXIS2_PLACEMENT_3D ( 'NONE', #8157, #7114, #1379 ) ;
#2414 =( BOUNDED_SURFACE ( )  B_SPLINE_SURFACE ( 1, 2, ( 
 ( #2874, #4810, #6804, #1943, #7851, #9713, #952, #6679, #1195, #4996, #1876, #2941, #3938, #6741, #2003, #8661, #4745, #11613, #3062, #2813, #3997, #6866, #11548, #10600, #1011, #9654, #7736, #1134, #5810, #2066, #4936, #5751, #8723, #6617, #8533, #3812, #10661, #2128, #7613, #9596, #2999, #1070, #11422, #9531, #184, #8783, #6925, #1253, #5061, #5991, #3122, #9779, #2180, #10720, #310, #8841, #4119, #11670, #3698, #4449, #10240, #11316, #12310, #12252, #9237 ),
 ( #2582, #5523, #1832, #10365, #10301, #3641, #10110, #723, #5642, #7507, #6569, #1652, #11190, #6515, #9419, #2762, #902, #5458, #4693, #655, #1770, #3581, #9298, #6449, #1590, #8486, #2526, #6389, #11065, #5393, #9174, #7448, #12130, #11254, #7389, #3760, #8247, #2642, #8308, #5581, #1715, #6326, #12068, #3524, #843, #7327, #785, #11126, #4572, #4516, #8366, #10177, #12193, #2703, #9359, #4635, #8428, #5765, #263, #1953, #9609, #2079, #136, #9545, #3076 ) ),
 .UNSPECIFIED., .F., .F., .F. ) 
 B_SPLINE_SURFACE_WITH_KNOTS ( ( 2, 2 ),
 ( 3, 2, 2, 2, 2, 2, 2, 2, 2, 2, 2, 2, 2, 2, 2, 2, 2, 2, 2, 2, 2, 2, 2, 2, 2, 2, 2, 2, 2, 2, 2, 2, 3 ),
 ( 0.000000000000000000, 1.000000000000000000 ),
 ( 0.000000000000000000, 0.03125000000000000000, 0.06250000000000000000, 0.09375000000000000000, 0.1250000000000000000, 0.1562500000000000000, 0.1875000000000000000, 0.2187500000000000000, 0.2500000000000000000, 0.2812500000000000000, 0.3125000000000000000, 0.3437500000000000000, 0.3750000000000000000, 0.4062500000000000000, 0.4375000000000000000, 0.4687500000000000000, 0.5000000000000000000, 0.5312500000000000000, 0.5625000000000000000, 0.5937500000000000000, 0.6250000000000000000, 0.6562500000000000000, 0.6875000000000000000, 0.7187500000000000000, 0.7500000000000000000, 0.7812500000000000000, 0.8125000000000000000, 0.8437500000000000000, 0.8750000000000000000, 0.9062500000000000000, 0.9375000000000000000, 0.9687500000000000000, 1.000000000000000000 ),
 .UNSPECIFIED. ) 
 GEOMETRIC_REPRESENTATION_ITEM ( )  RATIONAL_B_SPLINE_SURFACE ( (
 ( 1.000000000000000000, 0.9238795325112867385, 1.000000000000000000, 0.9238795325112867385, 1.000000000000000000, 0.9238795325112867385, 1.000000000000000000, 0.9238795325112867385, 1.000000000000000000, 0.9238795325112867385, 1.000000000000000000, 0.9238795325112867385, 1.000000000000000000, 0.9238795325112867385, 1.000000000000000000, 0.9238795325112867385, 1.000000000000000000, 0.9238795325112867385, 1.000000000000000000, 0.9238795325112867385, 1.000000000000000000, 0.9238795325112867385, 1.000000000000000000, 0.9238795325112867385, 1.000000000000000000, 0.9238795325112867385, 1.000000000000000000, 0.9238795325112867385, 1.000000000000000000, 0.9238795325112867385, 1.000000000000000000, 0.9238795325112867385, 1.000000000000000000, 0.9238795325112867385, 1.000000000000000000, 0.9238795325112867385, 1.000000000000000000, 0.9238795325112867385, 1.000000000000000000, 0.9238795325112867385, 1.000000000000000000, 0.9238795325112867385, 1.000000000000000000, 0.9238795325112867385, 1.000000000000000000, 0.9238795325112867385, 1.000000000000000000, 0.9238795325112867385, 1.000000000000000000, 0.9238795325112867385, 1.000000000000000000, 0.9238795325112867385, 1.000000000000000000, 0.9238795325112867385, 1.000000000000000000, 0.9238795325112867385, 1.000000000000000000, 0.9238795325112867385, 1.000000000000000000, 0.9238795325112867385, 1.000000000000000000, 0.9238795325112867385, 1.000000000000000000, 0.9238795325112867385, 1.000000000000000000),
 ( 1.000000000000000000, 0.9238795325112867385, 1.000000000000000000, 0.9238795325112867385, 1.000000000000000000, 0.9238795325112867385, 1.000000000000000000, 0.9238795325112867385, 1.000000000000000000, 0.9238795325112867385, 1.000000000000000000, 0.9238795325112867385, 1.000000000000000000, 0.9238795325112867385, 1.000000000000000000, 0.9238795325112867385, 1.000000000000000000, 0.9238795325112867385, 1.000000000000000000, 0.9238795325112867385, 1.000000000000000000, 0.9238795325112867385, 1.000000000000000000, 0.9238795325112867385, 1.000000000000000000, 0.9238795325112867385, 1.000000000000000000, 0.9238795325112867385, 1.000000000000000000, 0.9238795325112867385, 1.000000000000000000, 0.9238795325112867385, 1.000000000000000000, 0.9238795325112867385, 1.000000000000000000, 0.9238795325112867385, 1.000000000000000000, 0.9238795325112867385, 1.000000000000000000, 0.9238795325112867385, 1.000000000000000000, 0.9238795325112867385, 1.000000000000000000, 0.9238795325112867385, 1.000000000000000000, 0.9238795325112867385, 1.000000000000000000, 0.9238795325112867385, 1.000000000000000000, 0.9238795325112867385, 1.000000000000000000, 0.9238795325112867385, 1.000000000000000000, 0.9238795325112867385, 1.000000000000000000, 0.9238795325112867385, 1.000000000000000000, 0.9238795325112867385, 1.000000000000000000, 0.9238795325112867385, 1.000000000000000000, 0.9238795325112867385, 1.000000000000000000, 0.9238795325112867385, 1.000000000000000000) ) ) 
 REPRESENTATION_ITEM ( '' )  SURFACE ( )  );
#2415 = AXIS2_PLACEMENT_3D ( 'NONE', #6801, #9651, #244 ) ;
#2416 = EDGE_LOOP ( 'NONE', ( #6778, #2617, #12291, #4175 ) ) ;
#2417 = DIRECTION ( 'NONE',  ( 0.000000000000000000, 1.000000000000000000, 0.000000000000000000 ) ) ;
#2418 = VERTEX_POINT ( 'NONE', #1641 ) ;
#2419 = FACE_OUTER_BOUND ( 'NONE', #4288, .T. ) ;
#2420 = CARTESIAN_POINT ( 'NONE',  ( 5.453556438010031648, 41.17499691585408783, 80.00000048127353125 ) ) ;
#2421 = ORIENTED_EDGE ( 'NONE', *, *, #6395, .T. ) ;
#2422 = CIRCLE ( 'NONE', #1430, 105.0000000000000284 ) ;
#2423 = CARTESIAN_POINT ( 'NONE',  ( 170.0000000000011369, 230.0000000000000853, 20.00000000000000000 ) ) ;
#2424 = VECTOR ( 'NONE', #3740, 1000.000000000000000 ) ;
#2425 = CARTESIAN_POINT ( 'NONE',  ( -31.23312648697675797, 87.04033007153444146, -8.730107770814976575 ) ) ;
#2426 = EDGE_CURVE ( 'NONE', #9072, #8398, #11566, .T. ) ;
#2427 = EDGE_CURVE ( 'NONE', #3092, #11844, #774, .T. ) ;
#2428 = ORIENTED_EDGE ( 'NONE', *, *, #11053, .F. ) ;
#2429 = DIRECTION ( 'NONE',  ( -1.000000000000000000, 0.000000000000000000, 0.000000000000000000 ) ) ;
#2430 = EDGE_CURVE ( 'NONE', #9973, #9835, #3998, .T. ) ;
#2431 = EDGE_LOOP ( 'NONE', ( #7696, #7036, #9329, #5583 ) ) ;
#2432 = VECTOR ( 'NONE', #3576, 1000.000000000000000 ) ;
#2433 = DIRECTION ( 'NONE',  ( -1.000000000000000000, -0.000000000000000000, 0.000000000000000000 ) ) ;
#2434 = CARTESIAN_POINT ( 'NONE',  ( -2.298097038856279362, 114.2499999972688158, 2.298097038856279806 ) ) ;
#2435 = ORIENTED_EDGE ( 'NONE', *, *, #3268, .F. ) ;
#2436 = VERTEX_POINT ( 'NONE', #7439 ) ;
#2437 = CARTESIAN_POINT ( 'NONE',  ( -12.32411137850303184, 36.71650635094619730, 80.00000000000000000 ) ) ;
#2438 = CARTESIAN_POINT ( 'NONE',  ( 0.000000000000000000, 335.0000000000000000, 105.0000000000000284 ) ) ;
#2439 = ORIENTED_EDGE ( 'NONE', *, *, #3717, .F. ) ;
#2440 = ORIENTED_CLOSED_SHELL ( 'NONE', *, #12071, .F. );
#2441 = EDGE_CURVE ( 'NONE', #11288, #7839, #4685, .T. ) ;
#2442 =( BOUNDED_CURVE ( )  B_SPLINE_CURVE ( 3, ( #2458, #9233, #10403, #4513 ),
 .UNSPECIFIED., .F., .F. ) 
 B_SPLINE_CURVE_WITH_KNOTS ( ( 4, 4 ),
 ( 1.570796326794899000, 3.141592653589793116 ),
 .UNSPECIFIED. ) 
 CURVE ( )  GEOMETRIC_REPRESENTATION_ITEM ( )  RATIONAL_B_SPLINE_CURVE ( ( 1.000000000000000000, 0.8047378541243654926, 0.8047378541243654926, 1.000000000000000000 ) ) 
 REPRESENTATION_ITEM ( '' )  );
#2443 = CARTESIAN_POINT ( 'NONE',  ( 0.000000000000000000, 65.00000000000000000, 0.000000000000000000 ) ) ;
#2444 = DIRECTION ( 'NONE',  ( -0.8660254037844377084, 0.5000000000000015543, 0.000000000000000000 ) ) ;
#2445 = DIRECTION ( 'NONE',  ( 0.000000000000000000, 0.000000000000000000, -1.000000000000000000 ) ) ;
#2446 = VERTEX_POINT ( 'NONE', #4507 ) ;
#2447 = CARTESIAN_POINT ( 'NONE',  ( -1.121994411437818862, 110.8749999986343937, 2.708734124999999882 ) ) ;
#2448 = CIRCLE ( 'NONE', #11625, 9.999999999999994671 ) ;
#2449 = CARTESIAN_POINT ( 'NONE',  ( 70.93011667421329491, 17.92389934224341630, 24.58871393576433206 ) ) ;
#2450 = ORIENTED_EDGE ( 'NONE', *, *, #6316, .T. ) ;
#2451 = CARTESIAN_POINT ( 'NONE',  ( 75.70742691175847483, 15.93620156380750785, 22.92955197636053555 ) ) ;
#2452 = CYLINDRICAL_SURFACE ( 'NONE', #907, 100.0000000000000284 ) ;
#2453 = ORIENTED_EDGE ( 'NONE', *, *, #6299, .T. ) ;
#2454 = CARTESIAN_POINT ( 'NONE',  ( 0.000000000000000000, 65.00000000000000000, 0.000000000000000000 ) ) ;
#2455 = CARTESIAN_POINT ( 'NONE',  ( 71.26309188267669015, 48.71650692501490454, 23.38502809576078079 ) ) ;
#2456 = VECTOR ( 'NONE', #3663, 1000.000000000000000 ) ;
#2457 = ORIENTED_EDGE ( 'NONE', *, *, #11720, .T. ) ;
#2458 = CARTESIAN_POINT ( 'NONE',  ( 147.9289321881356045, 20.00000000000008527, -25.00000000000000000 ) ) ;
#2459 =( NAMED_UNIT ( * ) PLANE_ANGLE_UNIT ( ) SI_UNIT ( $, .RADIAN. ) );
#2460 = CARTESIAN_POINT ( 'NONE',  ( -4.975863863883684959E-16, 112.0624999986344079, -2.708734125000000326 ) ) ;
#2461 = EDGE_LOOP ( 'NONE', ( #4068, #8388 ) ) ;
#2462 =( NAMED_UNIT ( * ) PLANE_ANGLE_UNIT ( ) SI_UNIT ( $, .RADIAN. ) );
#2463 = ORIENTED_EDGE ( 'NONE', *, *, #7704, .T. ) ;
#2464 = AXIS2_PLACEMENT_3D ( 'NONE', #11019, #8892, #11905 ) ;
#2465 = ADVANCED_FACE ( 'NONE', ( #8298 ), #1802, .F. ) ;
#2466 = ADVANCED_FACE ( 'NONE', ( #6560 ), #4626, .T. ) ;
#2467 = CARTESIAN_POINT ( 'NONE',  ( 0.000000000000000000, 170.0000000000000000, 0.000000000000000000 ) ) ;
#2468 = DIRECTION ( 'NONE',  ( 0.000000000000000000, -1.000000000000000000, -0.000000000000000000 ) ) ;
#2470 = EDGE_CURVE ( 'NONE', #7137, #7682, #5448, .T. ) ;
#2469 = LINE ( 'NONE', #10816, #7444 ) ;
#2471 = CARTESIAN_POINT ( 'NONE',  ( 135.0000000000011084, 67.07106781186550393, -25.00000000000000000 ) ) ;
#2472 = CARTESIAN_POINT ( 'NONE',  ( 0.000000000000000000, 67.00000000000000000, 90.00000000000002842 ) ) ;
#2473 = CARTESIAN_POINT ( 'NONE',  ( 4.025725221640849227, 21.46474596215575659, 79.50000000000000000 ) ) ;
#2474 = DIRECTION ( 'NONE',  ( 0.000000000000000000, 0.000000000000000000, 1.000000000000000000 ) ) ;
#2475 = VECTOR ( 'NONE', #11753, 1000.000000000000000 ) ;
#2476 = DIRECTION ( 'NONE',  ( 1.000000000000000000, 0.000000000000000000, 0.000000000000000000 ) ) ;
#2477 = VECTOR ( 'NONE', #6418, 1000.000000000000000 ) ;
#2478 = CARTESIAN_POINT ( 'NONE',  ( 1.658621287961228566E-16, 113.5624999986344079, 2.708734125000000326 ) ) ;
#2479 = CARTESIAN_POINT ( 'NONE',  ( -2.708734124999999882, 111.0624999986344079, 3.317242575922456639E-16 ) ) ;
#2480 = CARTESIAN_POINT ( 'NONE',  ( -0.9407811293054709756, 40.00000000000008527, 79.50000000000000000 ) ) ;
#2481 = CARTESIAN_POINT ( 'NONE',  ( -1.024114462617946808, 43.00000000000008527, 80.00000048127353125 ) ) ;
#2482 = ORIENTED_EDGE ( 'NONE', *, *, #4520, .T. ) ;
#2483 = CARTESIAN_POINT ( 'NONE',  ( -8.500000000000000000, 165.5000000000000000, -6.164414002968973350 ) ) ;
#2484 = ORIENTED_EDGE ( 'NONE', *, *, #1751, .T. ) ;
#2485 = DIRECTION ( 'NONE',  ( -0.000000000000000000, -1.000000000000000000, -0.000000000000000000 ) ) ;
#2486 = CARTESIAN_POINT ( 'NONE',  ( 74.16198487095667247, 19.63704101494498744, -25.00000000000000355 ) ) ;
#2487 = ORIENTED_EDGE ( 'NONE', *, *, #10672, .T. ) ;
#2488 = CARTESIAN_POINT ( 'NONE',  ( -7.906085446029433861, 41.13124826485289276, 80.00000000000000000 ) ) ;
#2489 = CARTESIAN_POINT ( 'NONE',  ( 1.224646799147353375E-14, 265.0000000000000000, 100.0000000000000142 ) ) ;
#2490 = VECTOR ( 'NONE', #7158, 1000.000000000000114 ) ;
#2491 = ORIENTED_EDGE ( 'NONE', *, *, #7520, .T. ) ;
#2492 = CARTESIAN_POINT ( 'NONE',  ( 2.143131898507868248E-15, 87.50000000000000000, 17.50000000000000000 ) ) ;
#2493 = AXIS2_PLACEMENT_3D ( 'NONE', #5634, #2634, #8539 ) ;
#2494 = EDGE_CURVE ( 'NONE', #12345, #5565, #3580, .T. ) ;
#2495 = ORIENTED_EDGE ( 'NONE', *, *, #5948, .F. ) ;
#2496 = EDGE_CURVE ( 'NONE', #4895, #7265, #9751, .T. ) ;
#2497 = DIRECTION ( 'NONE',  ( 0.000000000000000000, 1.000000000000000000, 0.000000000000000000 ) ) ;
#2498 = ORIENTED_EDGE ( 'NONE', *, *, #6710, .T. ) ;
#2499 = AXIS2_PLACEMENT_3D ( 'NONE', #10697, #1352, #10818 ) ;
#2500 = ORIENTED_EDGE ( 'NONE', *, *, #10645, .T. ) ;
#2501 = DIRECTION ( 'NONE',  ( 0.000000000000000000, 0.000000000000000000, 1.000000000000000000 ) ) ;
#2502 = PLANE ( 'NONE',  #2307 ) ;
#2503 = ORIENTED_EDGE ( 'NONE', *, *, #6785, .F. ) ;
#2504 = VECTOR ( 'NONE', #1833, 1000.000000000000000 ) ;
#2505 = LINE ( 'NONE', #8160, #4894 ) ;
#2506 = CARTESIAN_POINT ( 'NONE',  ( 69.85388127645428824, 77.76794919243110371, -3.330127018922237614 ) ) ;
#2507 = PLANE ( 'NONE',  #11583 ) ;
#2508 = VERTEX_POINT ( 'NONE', #10293 ) ;
#2509 = CARTESIAN_POINT ( 'NONE',  ( 0.000000000000000000, 0.000000000000000000, 79.50000000000000000 ) ) ;
#2510 = CARTESIAN_POINT ( 'NONE',  ( 71.69575657208352482, 10.62176056569362537, 22.01828877003918450 ) ) ;
#2511 = AXIS2_PLACEMENT_3D ( 'NONE', #11634, #3083, #1094 ) ;
#2512 = EDGE_CURVE ( 'NONE', #12341, #7550, #10167, .T. ) ;
#2513 = EDGE_CURVE ( 'NONE', #2361, #6532, #8342, .T. ) ;
#2514 = CIRCLE ( 'NONE', #6297, 95.00000000000002842 ) ;
#2515 = ORIENTED_EDGE ( 'NONE', *, *, #8242, .F. ) ;
#2516 = FACE_BOUND ( 'NONE', #241, .T. ) ;
#2517 = CARTESIAN_POINT ( 'NONE',  ( 0.000000000000000000, 340.0000000000000000, -59.99999999999999289 ) ) ;
#2518 =( BOUNDED_CURVE ( )  B_SPLINE_CURVE ( 3, ( #2803, #3521, #7324, #11123 ),
 .UNSPECIFIED., .F., .F. ) 
 B_SPLINE_CURVE_WITH_KNOTS ( ( 4, 4 ),
 ( 4.419546208656112363, 5.005231752113266985 ),
 .UNSPECIFIED. ) 
 CURVE ( )  GEOMETRIC_REPRESENTATION_ITEM ( )  RATIONAL_B_SPLINE_CURVE ( ( 1.000000000000000000, 0.9716180718375584391, 0.9716180718375584391, 1.000000000000000000 ) ) 
 REPRESENTATION_ITEM ( '' )  );
#2519 = EDGE_LOOP ( 'NONE', ( #3043, #898, #6208, #10217 ) ) ;
#2520 = LINE ( 'NONE', #11999, #10828 ) ;
#2521 = CARTESIAN_POINT ( 'NONE',  ( 71.99731494077012428, 45.04006870689263309, 21.09170898385188408 ) ) ;
#2522 = VERTEX_POINT ( 'NONE', #5514 ) ;
#2523 = DIRECTION ( 'NONE',  ( -0.000000000000000000, 1.000000000000000000, -0.000000000000000000 ) ) ;
#2524 = LINE ( 'NONE', #1586, #6707 ) ;
#2525 = CARTESIAN_POINT ( 'NONE',  ( -1.121994411437820194, 111.9999999986343937, -2.708734124999999882 ) ) ;
#2526 = CARTESIAN_POINT ( 'NONE',  ( -1.915364268218909594, 112.1874999986344079, -1.915364268218908927 ) ) ;
#2527 = AXIS2_PLACEMENT_3D ( 'NONE', #11326, #2773, #5408 ) ;
#2528 = ORIENTED_EDGE ( 'NONE', *, *, #11945, .F. ) ;
#2529 = EDGE_LOOP ( 'NONE', ( #10134, #941, #10729, #6130, #6110, #9810, #9335, #11430, #3942 ) ) ;
#2530 = AXIS2_PLACEMENT_3D ( 'NONE', #720, #12128, #3637 ) ;
#2531 = CARTESIAN_POINT ( 'NONE',  ( -32.05000697088088657, 85.26794919243110371, -9.660254037844429931 ) ) ;
#2532 = DIRECTION ( 'NONE',  ( 0.000000000000000000, 0.000000000000000000, 1.000000000000000000 ) ) ;
#2533 = CARTESIAN_POINT ( 'NONE',  ( 0.000000000000000000, 75.00000000000001421, 0.000000000000000000 ) ) ;
#2534 = CARTESIAN_POINT ( 'NONE',  ( -27.96269517408193295, 86.23182228119658532, -11.42938571145656113 ) ) ;
#2535 = CARTESIAN_POINT ( 'NONE',  ( 11.80921887069467324, 30.25000000000018474, 79.50000000000000000 ) ) ;
#2536 = DIRECTION ( 'NONE',  ( 0.000000000000000000, 0.000000000000000000, 1.000000000000000000 ) ) ;
#2537 = CARTESIAN_POINT ( 'NONE',  ( 69.89773400907222367, 15.60145727894099288, -27.19132888315842678 ) ) ;
#2538 = ADVANCED_FACE ( 'NONE', ( #2516, #12121 ), #5633, .F. ) ;
#2539 = CARTESIAN_POINT ( 'NONE',  ( 1.346194077712559833, 111.8125000000000000, -3.250000000000000000 ) ) ;
#2540 = EDGE_CURVE ( 'NONE', #12227, #834, #8356, .T. ) ;
#2541 = CARTESIAN_POINT ( 'NONE',  ( 4.025725221640669815, 38.53525403784453118, 79.50000000000000000 ) ) ;
#2542 = CARTESIAN_POINT ( 'NONE',  ( 4.519788800730417222, 16.12168438296734152, 74.86496749433132436 ) ) ;
#2543 = ORIENTED_EDGE ( 'NONE', *, *, #9022, .T. ) ;
#2544 = FACE_OUTER_BOUND ( 'NONE', #8232, .T. ) ;
#2545 = FACE_OUTER_BOUND ( 'NONE', #2876, .T. ) ;
#2546 = CARTESIAN_POINT ( 'NONE',  ( 1.346194077712537629, 114.0624999972688016, 3.250000000000022649 ) ) ;
#2547 = ORIENTED_EDGE ( 'NONE', *, *, #1079, .F. ) ;
#2548 = APPLICATION_CONTEXT ( 'automotive_design' ) ;
#2549 = FACE_OUTER_BOUND ( 'NONE', #11279, .T. ) ;
#2550 = ADVANCED_FACE ( 'NONE', ( #11116 ), #3570, .T. ) ;
#2551 = CARTESIAN_POINT ( 'NONE',  ( 0.000000000000000000, 0.000000000000000000, 79.50000000000000000 ) ) ;
#2552 = VERTEX_POINT ( 'NONE', #12184 ) ;
#2553 = CARTESIAN_POINT ( 'NONE',  ( 0.000000000000000000, 335.0000000000000000, 0.000000000000000000 ) ) ;
#2554 = VERTEX_POINT ( 'NONE', #2571 ) ;
#2555 = LINE ( 'NONE', #5492, #8909 ) ;
#2556 = CARTESIAN_POINT ( 'NONE',  ( -1.190781129305471087, 30.00000000000008882, 65.00000000000000000 ) ) ;
#2557 = ORIENTED_EDGE ( 'NONE', *, *, #219, .F. ) ;
#2558 = DIRECTION ( 'NONE',  ( 1.000000000000000000, -0.000000000000000000, 1.224646799147353207E-16 ) ) ;
#2559 = CARTESIAN_POINT ( 'NONE',  ( -34.77127485704751564, 76.44489695195846934, 8.339765143629700006 ) ) ;
#2560 = VERTEX_POINT ( 'NONE', #1945 ) ;
#2561 = PRODUCT_DEFINITION_FORMATION_WITH_SPECIFIED_SOURCE ( 'ANY', '', #8763, .NOT_KNOWN. ) ;
#2562 = PLANE ( 'NONE',  #1081 ) ;
#2563 = DIRECTION ( 'NONE',  ( 1.000000000000000000, 0.000000000000000000, 0.000000000000000000 ) ) ;
#2564 = PLANE ( 'NONE',  #6000 ) ;
#2565 = EDGE_LOOP ( 'NONE', ( #6905, #5701, #7059, #11308 ) ) ;
#2566 = LINE ( 'NONE', #9222, #9544 ) ;
#2567 = EDGE_CURVE ( 'NONE', #1960, #3092, #8602, .T. ) ;
#2568 = CARTESIAN_POINT ( 'NONE',  ( 27.67899820261485999, 88.38261385519929547, 11.05501148229834030 ) ) ;
#2569 = ADVANCED_FACE ( 'NONE', ( #5814 ), #2068, .T. ) ;
#2570 = ORIENTED_EDGE ( 'NONE', *, *, #9023, .F. ) ;
#2571 = CARTESIAN_POINT ( 'NONE',  ( 100.7495955565343451, 275.0000000000000000, 29.57226733266770680 ) ) ;
#2572 = CARTESIAN_POINT ( 'NONE',  ( -12.32411137850302119, 23.28349364905396612, 80.00000000000000000 ) ) ;
#2573 = ORIENTED_EDGE ( 'NONE', *, *, #9688, .T. ) ;
#2574 = DIRECTION ( 'NONE',  ( 0.8660254037844420383, 0.4999999999999942824, 0.000000000000000000 ) ) ;
#2575 = LINE ( 'NONE', #9414, #5496 ) ;
#2576 = VERTEX_POINT ( 'NONE', #10540 ) ;
#2577 = CARTESIAN_POINT ( 'NONE',  ( 0.000000000000000000, 65.00000000000000000, 0.000000000000000000 ) ) ;
#2578 = CARTESIAN_POINT ( 'NONE',  ( 2.500000000000000000, -1.178949249685214307, 2.042000000000001592 ) ) ;
#2579 = CARTESIAN_POINT ( 'NONE',  ( 2.708734125000000326, 114.3124999986344079, 0.000000000000000000 ) ) ;
#2580 = VECTOR ( 'NONE', #5484, 1000.000000000000000 ) ;
#2581 = AXIS2_PLACEMENT_3D ( 'NONE', #2633, #8233, #12057 ) ;
#2582 = CARTESIAN_POINT ( 'NONE',  ( 2.708734124999999882, 110.5624999986344079, 0.000000000000000000 ) ) ;
#2583 = EDGE_CURVE ( 'NONE', #712, #5113, #4168, .T. ) ;
#2584 = ORIENTED_EDGE ( 'NONE', *, *, #982, .T. ) ;
#2585 = EDGE_CURVE ( 'NONE', #5113, #4639, #11142, .T. ) ;
#2586 = VECTOR ( 'NONE', #6126, 1000.000000000000000 ) ;
#2587 = DIRECTION ( 'NONE',  ( -1.000000000000000000, 6.938893903907222067E-15, 0.000000000000000000 ) ) ;
#2588 = DIRECTION ( 'NONE',  ( -0.000000000000000000, 1.000000000000000000, -0.000000000000000000 ) ) ;
#2589 = CARTESIAN_POINT ( 'NONE',  ( 9.942549119892413856, 23.28349364905404428, 80.00000000000000000 ) ) ;
#2590 = DIRECTION ( 'NONE',  ( 0.000000000000000000, 1.000000000000000000, 0.000000000000000000 ) ) ;
#2591 = AXIS2_PLACEMENT_3D ( 'NONE', #12353, #11489, #59 ) ;
#2592 = PLANE ( 'NONE',  #10054 ) ;
#2593 = CARTESIAN_POINT ( 'NONE',  ( 69.85388127645425982, 77.00000000000000000, -8.660254037844445918 ) ) ;
#2594 = CARTESIAN_POINT ( 'NONE',  ( 170.0000000000011369, 35.00000000000004974, -19.99999999999999645 ) ) ;
#2595 = EDGE_CURVE ( 'NONE', #10953, #6431, #2877, .T. ) ;
#2596 = ADVANCED_FACE ( 'NONE', ( #7556 ), #4940, .F. ) ;
#2597 = CARTESIAN_POINT ( 'NONE',  ( 69.62171139626217098, 17.74911263749020662, -27.88944765769274525 ) ) ;
#2598 = CARTESIAN_POINT ( 'NONE',  ( 1.346194077712559389, 111.1875000000000142, 3.250000000000000444 ) ) ;
#2599 = AXIS2_PLACEMENT_3D ( 'NONE', #2169, #7656, #10462 ) ;
#2600 = CARTESIAN_POINT ( 'NONE',  ( 2.708734125000000326, 110.3124999986344079, 0.000000000000000000 ) ) ;
#2601 = DIRECTION ( 'NONE',  ( -0.000000000000000000, -1.000000000000000000, -0.000000000000000000 ) ) ;
#2602 = VERTEX_POINT ( 'NONE', #2007 ) ;
#2603 = AXIS2_PLACEMENT_3D ( 'NONE', #1344, #276, #6830 ) ;
#2604 = LINE ( 'NONE', #1735, #8619 ) ;
#2605 = CARTESIAN_POINT ( 'NONE',  ( 0.000000000000000000, 50.00000000000000000, 0.000000000000000000 ) ) ;
#2606 = CARTESIAN_POINT ( 'NONE',  ( -12.44911137850311000, 23.50000000000024158, 80.00000000000000000 ) ) ;
#2607 = VERTEX_POINT ( 'NONE', #11365 ) ;
#2608 = LINE ( 'NONE', #9137, #2477 ) ;
#2609 = DIRECTION ( 'NONE',  ( -0.4999999999999942268, 0.8660254037844419273, 0.000000000000000000 ) ) ;
#2610 = EDGE_LOOP ( 'NONE', ( #10047, #6944, #9511, #1873 ) ) ;
#2611 = CARTESIAN_POINT ( 'NONE',  ( -14.19078112930532853, 30.25000000000008882, 79.50000000000000000 ) ) ;
#2612 = VECTOR ( 'NONE', #9033, 1000.000000000000000 ) ;
#2613 = ORIENTED_EDGE ( 'NONE', *, *, #7746, .F. ) ;
#2614 = EDGE_CURVE ( 'NONE', #5368, #5570, #8538, .T. ) ;
#2615 = CARTESIAN_POINT ( 'NONE',  ( 0.000000000000000000, 285.0000000000000568, 0.000000000000000000 ) ) ;
#2617 = ORIENTED_EDGE ( 'NONE', *, *, #2746, .T. ) ;
#2616 = CARTESIAN_POINT ( 'NONE',  ( 1.285879139104720633E-15, 122.5000000000000000, 10.49999999999999822 ) ) ;
#2618 = ORIENTED_EDGE ( 'NONE', *, *, #405, .F. ) ;
#2619 = DIRECTION ( 'NONE',  ( 0.8660254037844397068, 0.4999999999999981681, 0.000000000000000000 ) ) ;
#2620 = DIRECTION ( 'NONE',  ( 0.000000000000000000, -0.000000000000000000, 1.000000000000000000 ) ) ;
#2621 = AXIS2_PLACEMENT_3D ( 'NONE', #6498, #2684, #12234 ) ;
#2622 = EDGE_LOOP ( 'NONE', ( #6746, #7064, #6069, #9209 ) ) ;
#2623 = EDGE_CURVE ( 'NONE', #1747, #10667, #1589, .T. ) ;
#2624 = CARTESIAN_POINT ( 'NONE',  ( 0.000000000000000000, 0.000000000000000000, 0.000000000000000000 ) ) ;
#2625 = DIRECTION ( 'NONE',  ( -0.000000000000000000, -1.000000000000000000, -0.000000000000000000 ) ) ;
#2626 = FACE_OUTER_BOUND ( 'NONE', #678, .T. ) ;
#2627 = DIRECTION ( 'NONE',  ( 0.000000000000000000, 1.000000000000000000, 0.000000000000000000 ) ) ;
#2628 = ORIENTED_EDGE ( 'NONE', *, *, #8128, .T. ) ;
#2629 = CARTESIAN_POINT ( 'NONE',  ( 1.915364268218908705, 111.4374999986344079, -1.915364268218909594 ) ) ;
#2630 = CARTESIAN_POINT ( 'NONE',  ( -5.970153145843347347E-16, 113.7500000000000000, -3.250000000000000444 ) ) ;
#2631 = VERTEX_POINT ( 'NONE', #6868 ) ;
#2632 = ADVANCED_FACE ( 'NONE', ( #955, #1879 ), #7676, .F. ) ;
#2633 = CARTESIAN_POINT ( 'NONE',  ( 0.000000000000000000, 65.00000000000000000, 0.000000000000000000 ) ) ;
#2634 = DIRECTION ( 'NONE',  ( 0.000000000000000000, -1.000000000000000000, 0.000000000000000000 ) ) ;
#2635 = EDGE_LOOP ( 'NONE', ( #7285, #5878, #878, #11411 ) ) ;
#2636 = CARTESIAN_POINT ( 'NONE',  ( -3.250000000000000444, 112.4375000000000000, 1.346194077712559167 ) ) ;
#2637 = CARTESIAN_POINT ( 'NONE',  ( 72.04420248082804790, 49.75119935390800663, 20.85013644286522094 ) ) ;
#2638 = ORIENTED_EDGE ( 'NONE', *, *, #4576, .F. ) ;
#2639 = DIRECTION ( 'NONE',  ( 1.000000000000000000, 0.000000000000000000, -1.065814103640150437E-14 ) ) ;
#2640 = FACE_OUTER_BOUND ( 'NONE', #2416, .T. ) ;
#2641 = VECTOR ( 'NONE', #10061, 1000.000000000000000 ) ;
#2642 = CARTESIAN_POINT ( 'NONE',  ( -1.121994411437818862, 112.8749999986344079, 2.708734124999999882 ) ) ;
#2643 = EDGE_LOOP ( 'NONE', ( #5773, #6443, #6520, #10027 ) ) ;
#2644 = ORIENTED_EDGE ( 'NONE', *, *, #8199, .F. ) ;
#2645 = CIRCLE ( 'NONE', #6630, 17.00000000000000000 ) ;
#2646 = CARTESIAN_POINT ( 'NONE',  ( -1.440781129305282571, 17.00000000000009592, 80.00000000000000000 ) ) ;
#2647 = CARTESIAN_POINT ( 'NONE',  ( -25.00000000000000000, 347.0000000000000568, -59.99999999999999289 ) ) ;
#2648 = EDGE_CURVE ( 'NONE', #4148, #7445, #12302, .T. ) ;
#2649 = CARTESIAN_POINT ( 'NONE',  ( -32.15133482848810331, 77.00000000000000000, 7.827692000169491848 ) ) ;
#2650 = FACE_OUTER_BOUND ( 'NONE', #8310, .T. ) ;
#2651 = CARTESIAN_POINT ( 'NONE',  ( -1.440781129305471087, 40.00000000000008527, 80.00000000000000000 ) ) ;
#2652 = DIRECTION ( 'NONE',  ( 0.000000000000000000, -1.000000000000000000, 0.000000000000000000 ) ) ;
#2653 = FACE_BOUND ( 'NONE', #1467, .T. ) ;
#2654 = CARTESIAN_POINT ( 'NONE',  ( -3.250000000000001776, 112.5625000000000000, -1.346194077712558723 ) ) ;
#2655 = AXIS2_PLACEMENT_3D ( 'NONE', #11585, #10574, #2040 ) ;
#2656 = DIRECTION ( 'NONE',  ( 0.000000000000000000, 0.000000000000000000, -1.000000000000000000 ) ) ;
#2657 = ADVANCED_FACE ( 'NONE', ( #5934 ), #8665, .F. ) ;
#2658 = EDGE_CURVE ( 'NONE', #4082, #5298, #12340, .T. ) ;
#2659 = CARTESIAN_POINT ( 'NONE',  ( -0.9407811293054709756, 43.00000000000008527, 79.50000000000000000 ) ) ;
#2660 = ORIENTED_EDGE ( 'NONE', *, *, #8890, .F. ) ;
#2661 = LINE ( 'NONE', #6473, #1665 ) ;
#2662 = VECTOR ( 'NONE', #7873, 1000.000000000000000 ) ;
#2663 = AXIS2_PLACEMENT_3D ( 'NONE', #442, #5251, #3193 ) ;
#2664 = CARTESIAN_POINT ( 'NONE',  ( 0.000000000000000000, 0.000000000000000000, 79.50000000000000000 ) ) ;
#2665 = CARTESIAN_POINT ( 'NONE',  ( 70.93313137955964010, 17.93151681614107318, -24.57887570927868026 ) ) ;
#2666 = ORIENTED_EDGE ( 'NONE', *, *, #8899, .T. ) ;
#2667 = CARTESIAN_POINT ( 'NONE',  ( 1.200153863164406345E-14, 75.00000000000001421, 98.00000000000001421 ) ) ;
#2668 = DIRECTION ( 'NONE',  ( -0.000000000000000000, -1.000000000000000000, -0.000000000000000000 ) ) ;
#2669 = EDGE_LOOP ( 'NONE', ( #6979, #8099, #1828, #6259 ) ) ;
#2670 = DIRECTION ( 'NONE',  ( 0.000000000000000000, 1.000000000000000000, 0.000000000000000000 ) ) ;
#2671 = AXIS2_PLACEMENT_3D ( 'NONE', #2454, #6195, #8986 ) ;
#2672 = VECTOR ( 'NONE', #349, 1000.000000000000114 ) ;
#2673 = ORIENTED_EDGE ( 'NONE', *, *, #5949, .F. ) ;
#2674 = CARTESIAN_POINT ( 'NONE',  ( 0.000000000000000000, 165.5000000000000000, 0.000000000000000000 ) ) ;
#2676 = ORIENTED_EDGE ( 'NONE', *, *, #5111, .T. ) ;
#2675 = LINE ( 'NONE', #8339, #9004 ) ;
#2677 = ORIENTED_EDGE ( 'NONE', *, *, #11274, .T. ) ;
#2678 = CARTESIAN_POINT ( 'NONE',  ( -17.30235457177319347, 275.0000000000000000, -113.6909342308024549 ) ) ;
#2679 = DIRECTION ( 'NONE',  ( 0.000000000000000000, 0.4999999999999992784, -0.8660254037844389297 ) ) ;
#2680 = EDGE_LOOP ( 'NONE', ( #2482, #1202, #8792, #10721, #2255, #1406 ) ) ;
#2681 = AXIS2_PLACEMENT_3D ( 'NONE', #11662, #3113, #7033 ) ;
#2682 = DIRECTION ( 'NONE',  ( -1.000000000000000000, 0.000000000000000000, -3.469446951953613203E-16 ) ) ;
#2683 = AXIS2_PLACEMENT_3D ( 'NONE', #10168, #1642, #5449 ) ;
#2684 = DIRECTION ( 'NONE',  ( 0.000000000000000000, -0.4999999999999965028, -0.8660254037844407060 ) ) ;
#2685 = CARTESIAN_POINT ( 'NONE',  ( 2.500000000000000000, -1.178949249685214307, 2.042000000000001592 ) ) ;
#2686 = ORIENTED_EDGE ( 'NONE', *, *, #7352, .T. ) ;
#2687 = CARTESIAN_POINT ( 'NONE',  ( 2.708734124999999882, 113.6249999986344079, 1.121994411437818862 ) ) ;
#2688 = EDGE_CURVE ( 'NONE', #544, #5668, #5175, .T. ) ;
#2689 = EDGE_CURVE ( 'NONE', #3929, #8835, #3749, .T. ) ;
#2690 = DIRECTION ( 'NONE',  ( -0.000000000000000000, -0.000000000000000000, 1.000000000000000000 ) ) ;
#2691 = EDGE_CURVE ( 'NONE', #9973, #8106, #10416, .T. ) ;
#2692 = VECTOR ( 'NONE', #7887, 1000.000000000000114 ) ;
#2693 = VERTEX_POINT ( 'NONE', #11425 ) ;
#2694 = CARTESIAN_POINT ( 'NONE',  ( 0.000000000000000000, 67.00000000000000000, 0.000000000000000000 ) ) ;
#2695 = CARTESIAN_POINT ( 'NONE',  ( 69.62171139626212835, 42.25088736250997101, 27.88944765769274170 ) ) ;
#2696 = ORIENTED_EDGE ( 'NONE', *, *, #7107, .F. ) ;
#2697 = CARTESIAN_POINT ( 'NONE',  ( -3.250000000000000444, 112.5000000000000000, 3.980102097228898231E-16 ) ) ;
#2698 = CARTESIAN_POINT ( 'NONE',  ( -20.00000000000004263, 54.99999999999999289, 67.08203932499370126 ) ) ;
#2699 = ORIENTED_EDGE ( 'NONE', *, *, #2131, .T. ) ;
#2700 = CARTESIAN_POINT ( 'NONE',  ( -17.30235457177319347, 285.0000000000000568, -113.6909342308024549 ) ) ;
#2701 = DIRECTION ( 'NONE',  ( -0.7071067811865464625, 0.7071067811865486830, 2.453269466693394184E-16 ) ) ;
#2702 = AXIS2_PLACEMENT_3D ( 'NONE', #974, #4763, #10183 ) ;
#2703 = CARTESIAN_POINT ( 'NONE',  ( -1.121994411437818862, 113.8749999986343937, 2.708734124999999882 ) ) ;
#2704 = CARTESIAN_POINT ( 'NONE',  ( 2.708734124999999882, 111.5624999986344079, 0.000000000000000000 ) ) ;
#2705 = ORIENTED_EDGE ( 'NONE', *, *, #7052, .T. ) ;
#2706 = ORIENTED_EDGE ( 'NONE', *, *, #7986, .F. ) ;
#2707 = APPLICATION_PROTOCOL_DEFINITION ( 'draft international standard', 'automotive_design', 1998, #8674 ) ;
#2708 = AXIS2_PLACEMENT_3D ( 'NONE', #5329, #9170, #11185 ) ;
#2709 = LINE ( 'NONE', #7571, #6453 ) ;
#2710 = LINE ( 'NONE', #3706, #8120 ) ;
#2711 = ORIENTED_EDGE ( 'NONE', *, *, #953, .T. ) ;
#2712 = CARTESIAN_POINT ( 'NONE',  ( -7.473072744137207124, 41.38124826485288565, 80.00000000000000000 ) ) ;
#2713 = DIRECTION ( 'NONE',  ( 0.000000000000000000, 1.000000000000000000, 0.000000000000000000 ) ) ;
#2714 = AXIS2_PLACEMENT_3D ( 'NONE', #2391, #7879, #524 ) ;
#2715 = LINE ( 'NONE', #3886, #9451 ) ;
#2716 = CARTESIAN_POINT ( 'NONE',  ( -14.19078112930533209, 29.75000000000008882, 80.00000000000000000 ) ) ;
#2717 = DIRECTION ( 'NONE',  ( -1.000000000000000000, 3.469446951953611033E-15, 0.000000000000000000 ) ) ;
#2718 = CYLINDRICAL_SURFACE ( 'NONE', #8556, 110.0000000000000284 ) ;
#2719 = EDGE_CURVE ( 'NONE', #5158, #590, #9658, .T. ) ;
#2720 = AXIS2_PLACEMENT_3D ( 'NONE', #2271, #8057, #2211 ) ;
#2721 = EDGE_CURVE ( 'NONE', #7739, #5487, #9535, .T. ) ;
#2722 = CARTESIAN_POINT ( 'NONE',  ( 3.645076725190190992, 15.79321527920849633, 74.91265089688103274 ) ) ;
#2723 = CARTESIAN_POINT ( 'NONE',  ( -7.907287480251413925, 18.86666975080236597, 80.00000000000000000 ) ) ;
#2724 = ORIENTED_EDGE ( 'NONE', *, *, #7617, .F. ) ;
#2725 = CARTESIAN_POINT ( 'NONE',  ( -1.190781129305471087, 30.00000000000008882, 80.00000000000000000 ) ) ;
#2726 = CARTESIAN_POINT ( 'NONE',  ( -8.000000000000000000, 165.0000000000000000, -5.999999999999998224 ) ) ;
#2727 = CARTESIAN_POINT ( 'NONE',  ( 69.73318542092266625, 16.71298883719501305, -27.60965287711918492 ) ) ;
#2728 = ORIENTED_EDGE ( 'NONE', *, *, #2745, .F. ) ;
#2729 = DIRECTION ( 'NONE',  ( 0.000000000000000000, 1.000000000000000000, 0.000000000000000000 ) ) ;
#2730 = CARTESIAN_POINT ( 'NONE',  ( 0.2500000000000002220, 0.000000000000000000, 0.000000000000000000 ) ) ;
#2731 = ORIENTED_EDGE ( 'NONE', *, *, #937, .T. ) ;
#2732 = EDGE_CURVE ( 'NONE', #3744, #2602, #4767, .T. ) ;
#2733 = CARTESIAN_POINT ( 'NONE',  ( 145.0000000000011369, 225.0000000000000853, -20.00000000000000000 ) ) ;
#2734 = EDGE_CURVE ( 'NONE', #3401, #4827, #6363, .T. ) ;
#2735 = ORIENTED_EDGE ( 'NONE', *, *, #1498, .T. ) ;
#2736 = DIRECTION ( 'NONE',  ( 0.000000000000000000, 0.5150380749100502698, 0.8571673007021147761 ) ) ;
#2737 = FACE_OUTER_BOUND ( 'NONE', #6486, .T. ) ;
#2738 = VERTEX_POINT ( 'NONE', #7047 ) ;
#2739 = DIRECTION ( 'NONE',  ( 0.000000000000000000, 1.000000000000000000, 0.000000000000000000 ) ) ;
#2740 = ORIENTED_EDGE ( 'NONE', *, *, #9346, .T. ) ;
#2741 = DIRECTION ( 'NONE',  ( -3.469446951953613203E-16, 0.000000000000000000, 1.000000000000000000 ) ) ;
#2742 = DIRECTION ( 'NONE',  ( -0.000000000000000000, 0.4999999999999965028, 0.8660254037844407060 ) ) ;
#2743 = SPHERICAL_SURFACE ( 'NONE', #4803, 5.000000000000000000 ) ;
#2744 = CIRCLE ( 'NONE', #7733, 10.00000000000000888 ) ;
#2745 = EDGE_CURVE ( 'NONE', #6757, #1244, #4738, .T. ) ;
#2746 = EDGE_CURVE ( 'NONE', #5955, #11632, #8787, .T. ) ;
#2747 = VERTEX_POINT ( 'NONE', #313 ) ;
#2748 = CARTESIAN_POINT ( 'NONE',  ( -1.121994411437820194, 111.2499999986344079, -2.708734124999999437 ) ) ;
#2749 = CARTESIAN_POINT ( 'NONE',  ( 4.163799117101000559E-16, 115.0000000000000000, -3.399999999999999911 ) ) ;
#2750 = ORIENTED_EDGE ( 'NONE', *, *, #1431, .F. ) ;
#2751 = VECTOR ( 'NONE', #12258, 1000.000000000000000 ) ;
#2752 = DIRECTION ( 'NONE',  ( 6.938893903907228378E-17, 0.000000000000000000, -1.000000000000000000 ) ) ;
#2753 = CARTESIAN_POINT ( 'NONE',  ( -15.76450185945197902, 26.41238025498855180, 73.32456738963179532 ) ) ;
#2754 = VERTEX_POINT ( 'NONE', #7170 ) ;
#2755 = CARTESIAN_POINT ( 'NONE',  ( 0.000000000000000000, 285.0000000000000568, 100.0000000000000284 ) ) ;
#2756 = LINE ( 'NONE', #9168, #4692 ) ;
#2757 = ORIENTED_EDGE ( 'NONE', *, *, #4392, .T. ) ;
#2758 = PRODUCT_RELATED_PRODUCT_CATEGORY ( 'part', '', ( #102 ) ) ;
#2759 = EDGE_CURVE ( 'NONE', #2264, #334, #11255, .T. ) ;
#2760 = LINE ( 'NONE', #6387, #8487 ) ;
#2761 = DIRECTION ( 'NONE',  ( -1.000000000000000000, -0.000000000000000000, -0.000000000000000000 ) ) ;
#2762 = CARTESIAN_POINT ( 'NONE',  ( 2.708734124999999437, 111.4999999986343937, -1.121994411437820638 ) ) ;
#2763 = CARTESIAN_POINT ( 'NONE',  ( -20.00000000000000355, 50.00000000000000000, -57.08203932499370836 ) ) ;
#2764 = ORIENTED_EDGE ( 'NONE', *, *, #1822, .F. ) ;
#2765 =( NAMED_UNIT ( * ) PLANE_ANGLE_UNIT ( ) SI_UNIT ( $, .RADIAN. ) );
#2766 = EDGE_CURVE ( 'NONE', #1112, #11439, #1439, .T. ) ;
#2767 = DIRECTION ( 'NONE',  ( 0.000000000000000000, 0.000000000000000000, 1.000000000000000000 ) ) ;
#2768 = VERTEX_POINT ( 'NONE', #5066 ) ;
#2769 = CARTESIAN_POINT ( 'NONE',  ( 13.80921887069452758, 30.00000000000009237, 80.00000000000000000 ) ) ;
#2770 = CIRCLE ( 'NONE', #10938, 30.00000000000000355 ) ;
#2771 = AXIS2_PLACEMENT_3D ( 'NONE', #10562, #4768, #24 ) ;
#2772 = CYLINDRICAL_SURFACE ( 'NONE', #10557, 9.999999999999994671 ) ;
#2773 = DIRECTION ( 'NONE',  ( 0.000000000000000000, 1.000000000000000000, 0.000000000000000000 ) ) ;
#2774 = DIRECTION ( 'NONE',  ( 0.000000000000000000, 1.000000000000000000, 0.000000000000000000 ) ) ;
#2775 = B_SPLINE_CURVE_WITH_KNOTS ( 'NONE', 3,
 ( #1617, #6538, #6352, #10325 ),
 .UNSPECIFIED., .F., .F.,
 ( 4, 4 ),
 ( 0.000000000000000000, 0.001357209897699809299 ),
 .UNSPECIFIED. ) ;
#2776 = DIRECTION ( 'NONE',  ( 0.5000000000000039968, 0.000000000000000000, -0.8660254037844363761 ) ) ;
#2777 = AXIS2_PLACEMENT_3D ( 'NONE', #11528, #1178, #4920 ) ;
#2778 =( GEOMETRIC_REPRESENTATION_CONTEXT ( 3 ) GLOBAL_UNCERTAINTY_ASSIGNED_CONTEXT ( ( #5276 ) ) GLOBAL_UNIT_ASSIGNED_CONTEXT ( ( #5723, #4777, #10510 ) ) REPRESENTATION_CONTEXT ( 'NONE', 'WORKASPACE' ) );
#2779 = UNCERTAINTY_MEASURE_WITH_UNIT (LENGTH_MEASURE( 1.000000000000000082E-05 ), #12007, 'distance_accuracy_value', 'NONE');
#2780 = CARTESIAN_POINT ( 'NONE',  ( 76.47547367680522257, 44.68911971724172361, -21.74308734404387167 ) ) ;
#2781 = FACE_OUTER_BOUND ( 'NONE', #6057, .T. ) ;
#2782 = ORIENTED_EDGE ( 'NONE', *, *, #8591, .F. ) ;
#2783 = DIRECTION ( 'NONE',  ( 0.000000000000000000, 0.000000000000000000, 1.000000000000000000 ) ) ;
#2784 = CARTESIAN_POINT ( 'NONE',  ( 3.249999999999999556, 112.9375000000000000, -1.346194077712561166 ) ) ;
#2785 = DIRECTION ( 'NONE',  ( -1.000000000000000000, 0.000000000000000000, 0.000000000000000000 ) ) ;
#2786 = VERTEX_POINT ( 'NONE', #6055 ) ;
#2787 = EDGE_CURVE ( 'NONE', #10587, #5507, #5939, .T. ) ;
#2788 = AXIS2_PLACEMENT_3D ( 'NONE', #1329, #6997, #3952 ) ;
#2789 = CARTESIAN_POINT ( 'NONE',  ( 8.939921633775681592E-15, 52.00000000000000711, 73.00000000000002842 ) ) ;
#2790 = PRODUCT_DEFINITION_SHAPE ( 'NONE', 'NONE',  #545 ) ;
#2791 = EDGE_CURVE ( 'NONE', #11350, #11684, #2744, .T. ) ;
#2792 = CARTESIAN_POINT ( 'NONE',  ( -8.000000000000000000, 165.0000000000000000, 5.999999999999998224 ) ) ;
#2793 = ORIENTED_EDGE ( 'NONE', *, *, #5485, .T. ) ;
#2794 = CARTESIAN_POINT ( 'NONE',  ( -31.74999999999995737, 0.000000000000000000, 0.000000000000000000 ) ) ;
#2795 = VECTOR ( 'NONE', #3014, 1000.000000000000000 ) ;
#2796 = AXIS2_PLACEMENT_3D ( 'NONE', #9436, #4652, #2776 ) ;
#2797 = AXIS2_PLACEMENT_3D ( 'NONE', #1841, #85, #2838 ) ;
#2798 = ORIENTED_EDGE ( 'NONE', *, *, #5540, .F. ) ;
#2799 = CARTESIAN_POINT ( 'NONE',  ( 41.03553390593252459, -41.03553390593295802, 25.00000000000000000 ) ) ;
#2800 = FACE_OUTER_BOUND ( 'NONE', #2529, .T. ) ;
#2801 = ORIENTED_EDGE ( 'NONE', *, *, #10352, .F. ) ;
#2802 = CARTESIAN_POINT ( 'NONE',  ( 0.000000000000000000, 65.00000000000000000, -70.00000000000001421 ) ) ;
#2803 = CARTESIAN_POINT ( 'NONE',  ( -28.72281323269012887, 87.00000000000000000, -8.660254037844435260 ) ) ;
#2804 = EDGE_LOOP ( 'NONE', ( #12277, #1128, #3707, #3241 ) ) ;
#2805 = ADVANCED_FACE ( 'NONE', ( #7970 ), #5245, .T. ) ;
#2806 = EDGE_CURVE ( 'NONE', #2508, #945, #10970, .T. ) ;
#2807 = DIRECTION ( 'NONE',  ( -0.000000000000000000, -1.000000000000000000, 0.000000000000000000 ) ) ;
#2809 = CARTESIAN_POINT ( 'NONE',  ( -31.88521078284829713, 86.99999999999998579, -14.43375672974068991 ) ) ;
#2808 = AXIS2_PLACEMENT_3D ( 'NONE', #9218, #9469, #12296 ) ;
#2810 = CARTESIAN_POINT ( 'NONE',  ( 165.0000000000011369, 225.0000000000000853, -20.00000000000000000 ) ) ;
#2811 = ORIENTED_EDGE ( 'NONE', *, *, #4159, .F. ) ;
#2812 = CARTESIAN_POINT ( 'NONE',  ( -2.708734125000000326, 114.1249999986344079, -1.121994411437818195 ) ) ;
#2813 = CARTESIAN_POINT ( 'NONE',  ( 1.346194077712559389, 112.0624999972688016, 3.250000000000000444 ) ) ;
#2814 = AXIS2_PLACEMENT_3D ( 'NONE', #4066, #190, #5937 ) ;
#2815 = AXIS2_PLACEMENT_3D ( 'NONE', #8319, #6151, #11010 ) ;
#2816 = VERTEX_POINT ( 'NONE', #8963 ) ;
#2817 = ADVANCED_FACE ( 'NONE', ( #436 ), #8031, .F. ) ;
#2818 = DIRECTION ( 'NONE',  ( 0.000000000000000000, 1.000000000000000000, 0.000000000000000000 ) ) ;
#2819 = EDGE_CURVE ( 'NONE', #11587, #7445, #10029, .T. ) ;
#2820 = CARTESIAN_POINT ( 'NONE',  ( 71.66575360104040726, 49.33907185937723483, 22.11578253505649982 ) ) ;
#2821 = ORIENTED_EDGE ( 'NONE', *, *, #12269, .T. ) ;
#2822 = CARTESIAN_POINT ( 'NONE',  ( 0.000000000000000000, 110.0000000000000000, 0.000000000000000000 ) ) ;
#2823 = DIRECTION ( 'NONE',  ( 1.000000000000000000, 0.000000000000000000, 0.000000000000000000 ) ) ;
#2824 = ORIENTED_EDGE ( 'NONE', *, *, #304, .F. ) ;
#2825 = DIRECTION ( 'NONE',  ( -1.000000000000000000, -0.000000000000000000, -0.000000000000000000 ) ) ;
#2826 = FACE_BOUND ( 'NONE', #7544, .T. ) ;
#2827 = CARTESIAN_POINT ( 'NONE',  ( -25.00000000000000000, 445.0000000000000568, -24.99999999999998934 ) ) ;
#2828 = AXIS2_PLACEMENT_3D ( 'NONE', #1968, #3774, #2840 ) ;
#2829 = CARTESIAN_POINT ( 'NONE',  ( 0.000000000000000000, 67.00000000000000000, 0.000000000000000000 ) ) ;
#2830 = ADVANCED_FACE ( 'NONE', ( #6928 ), #10724, .F. ) ;
#2831 = EDGE_LOOP ( 'NONE', ( #7123, #8086, #11427, #1508 ) ) ;
#2832 = FILL_AREA_STYLE ('',( #5769 ) ) ;
#2833 = ORIENTED_EDGE ( 'NONE', *, *, #1657, .F. ) ;
#2834 = CARTESIAN_POINT ( 'NONE',  ( -9.976035167149731819, 34.78349364905394481, 79.50000000000000000 ) ) ;
#2835 = AXIS2_PLACEMENT_3D ( 'NONE', #6137, #6950, #1219 ) ;
#2836 = ORIENTED_EDGE ( 'NONE', *, *, #2426, .T. ) ;
#2837 = CARTESIAN_POINT ( 'NONE',  ( 25.00000000000000000, 445.0000000000000568, -59.99999999999999289 ) ) ;
#2838 = DIRECTION ( 'NONE',  ( 0.000000000000000000, 0.000000000000000000, -1.000000000000000000 ) ) ;
#2839 = CARTESIAN_POINT ( 'NONE',  ( 1.836970198721029589E-15, 75.00000000000000000, 15.00000000000000000 ) ) ;
#2840 = DIRECTION ( 'NONE',  ( 0.4999999999999985567, -0.8660254037844394848, 0.000000000000000000 ) ) ;
#2841 =( BOUNDED_CURVE ( )  B_SPLINE_CURVE ( 3, ( #8964, #1746, #3616, #3799 ),
 .UNSPECIFIED., .F., .F. ) 
 B_SPLINE_CURVE_WITH_KNOTS ( ( 4, 4 ),
 ( 4.419546208656112363, 5.005231752113266985 ),
 .UNSPECIFIED. ) 
 CURVE ( )  GEOMETRIC_REPRESENTATION_ITEM ( )  RATIONAL_B_SPLINE_CURVE ( ( 1.000000000000000000, 0.9716180718375584391, 0.9716180718375584391, 1.000000000000000000 ) ) 
 REPRESENTATION_ITEM ( '' )  );
#2842 = VERTEX_POINT ( 'NONE', #6301 ) ;
#2843 = EDGE_CURVE ( 'NONE', #3680, #4047, #8403, .T. ) ;
#2844 = EDGE_CURVE ( 'NONE', #4062, #7080, #11713, .T. ) ;
#2845 = CIRCLE ( 'NONE', #1461, 5.000000000000001776 ) ;
#2846 = EDGE_CURVE ( 'NONE', #7525, #7634, #1957, .T. ) ;
#2847 = CARTESIAN_POINT ( 'NONE',  ( 71.30804307394106445, 43.76264759282432237, -23.42323195207071507 ) ) ;
#2848 = DIRECTION ( 'NONE',  ( -1.040834085586083310E-14, -1.000000000000000000, 0.000000000000000000 ) ) ;
#2849 = ORIENTED_EDGE ( 'NONE', *, *, #11264, .T. ) ;
#2850 = DIRECTION ( 'NONE',  ( -0.4999999999999933387, 0.8660254037844424824, 0.000000000000000000 ) ) ;
#2851 = DIRECTION ( 'NONE',  ( 0.000000000000000000, 1.000000000000000000, 0.000000000000000000 ) ) ;
#2852 = CARTESIAN_POINT ( 'NONE',  ( -12.57411137850301763, 23.71650635094618664, 80.00000000000000000 ) ) ;
#2853 = EDGE_LOOP ( 'NONE', ( #3610, #6946, #1825, #10648 ) ) ;
#2854 = DIRECTION ( 'NONE',  ( -0.000000000000000000, 1.000000000000000000, -0.000000000000000000 ) ) ;
#2855 = ORIENTED_EDGE ( 'NONE', *, *, #10409, .F. ) ;
#2856 = CARTESIAN_POINT ( 'NONE',  ( 0.000000000000000000, 122.0000000000000000, 17.00000000000000000 ) ) ;
#2857 = CIRCLE ( 'NONE', #4069, 0.2500000000000002220 ) ;
#2858 = VECTOR ( 'NONE', #10914, 1000.000000000000000 ) ;
#2859 = EDGE_LOOP ( 'NONE', ( #11635, #11057, #12176, #7298 ) ) ;
#2860 = CARTESIAN_POINT ( 'NONE',  ( 2.500000000000000000, 1.178949249685212974, -2.042000000000001148 ) ) ;
#2861 = FACE_OUTER_BOUND ( 'NONE', #5513, .T. ) ;
#2862 = EDGE_LOOP ( 'NONE', ( #2918, #6840 ) ) ;
#2863 = CARTESIAN_POINT ( 'NONE',  ( 30.98881549816775660, 77.00000000000001421, -6.657310619789788220 ) ) ;
#2864 = DIRECTION ( 'NONE',  ( 0.000000000000000000, -0.5000000000000009992, -0.8660254037844380415 ) ) ;
#2865 = EDGE_LOOP ( 'NONE', ( #7611, #6742, #1849, #9784, #12183, #7498, #56, #6864, #6783, #318 ) ) ;
#2866 = DIRECTION ( 'NONE',  ( 6.123233995736766036E-17, -1.000000000000000000, 0.000000000000000000 ) ) ;
#2867 = FACE_OUTER_BOUND ( 'NONE', #8250, .T. ) ;
#2868 = FACE_BOUND ( 'NONE', #2680, .T. ) ;
#2869 = DIRECTION ( 'NONE',  ( 0.000000000000000000, 1.000000000000000000, 0.000000000000000000 ) ) ;
#2870 = AXIS2_PLACEMENT_3D ( 'NONE', #6382, #7190, #10992 ) ;
#2871 = ORIENTED_EDGE ( 'NONE', *, *, #10993, .F. ) ;
#2872 = CARTESIAN_POINT ( 'NONE',  ( 2.708734124999999882, 112.6249999986343937, 1.121994411437818862 ) ) ;
#2873 = AXIS2_PLACEMENT_3D ( 'NONE', #8702, #10456, #9697 ) ;
#2874 = CARTESIAN_POINT ( 'NONE',  ( 3.250000000000000444, 110.8749999972688158, 0.000000000000000000 ) ) ;
#2875 = EDGE_CURVE ( 'NONE', #4551, #4695, #8510, .T. ) ;
#2876 = EDGE_LOOP ( 'NONE', ( #9275, #4841, #9522, #3365 ) ) ;
#2877 = LINE ( 'NONE', #62, #5369 ) ;
#2878 = CARTESIAN_POINT ( 'NONE',  ( -12.57411137850301763, 23.71650635094618664, 80.00000000000000000 ) ) ;
#2879 = AXIS2_PLACEMENT_3D ( 'NONE', #7305, #9337, #879 ) ;
#2880 = VERTEX_POINT ( 'NONE', #9147 ) ;
#2881 = DIRECTION ( 'NONE',  ( -1.000000000000000000, -0.000000000000000000, -0.000000000000000000 ) ) ;
#2882 = CARTESIAN_POINT ( 'NONE',  ( 69.71747094087791652, 16.79237370886442804, 27.65023488237563498 ) ) ;
#2883 = ORIENTED_EDGE ( 'NONE', *, *, #10339, .T. ) ;
#2884 = LINE ( 'NONE', #2015, #10279 ) ;
#2885 = CARTESIAN_POINT ( 'NONE',  ( 10.19254911989230727, 36.28349364905406560, 80.00000000000000000 ) ) ;
#2886 = DIRECTION ( 'NONE',  ( 0.000000000000000000, 0.000000000000000000, -1.000000000000000000 ) ) ;
#2887 = CARTESIAN_POINT ( 'NONE',  ( 1.990051048614449116E-16, 113.2500000000000000, 3.250000000000000444 ) ) ;
#2888 = EDGE_CURVE ( 'NONE', #8670, #4839, #1756, .T. ) ;
#2889 = CARTESIAN_POINT ( 'NONE',  ( -2.708734125000000326, 114.1249999986344079, -1.121994411437818195 ) ) ;
#2890 = VECTOR ( 'NONE', #7348, 1000.000000000000000 ) ;
#2891 = ORIENTED_EDGE ( 'NONE', *, *, #11765, .T. ) ;
#2892 = EDGE_CURVE ( 'NONE', #8933, #8398, #3945, .T. ) ;
#2893 = SURFACE_SIDE_STYLE ('',( #6634 ) ) ;
#2894 = AXIS2_PLACEMENT_3D ( 'NONE', #2176, #117, #4992 ) ;
#2895 = ORIENTED_EDGE ( 'NONE', *, *, #9499, .T. ) ;
#2896 = STYLED_ITEM ( 'NONE', ( #10572 ), #482 ) ;
#2897 = CARTESIAN_POINT ( 'NONE',  ( -7.907287480251421030, 41.13333024919781167, 79.50000000000000000 ) ) ;
#2898 = CARTESIAN_POINT ( 'NONE',  ( 3.197275507839122177, 44.35135159419116491, 74.93316431128972965 ) ) ;
#2899 = EDGE_LOOP ( 'NONE', ( #8408, #5265, #5179, #1687 ) ) ;
#2900 = FACE_BOUND ( 'NONE', #8062, .T. ) ;
#2901 = MECHANICAL_DESIGN_GEOMETRIC_PRESENTATION_REPRESENTATION (  '', ( #10655 ), #9649 ) ;
#2902 = DIRECTION ( 'NONE',  ( -0.000000000000000000, -1.000000000000000000, -0.000000000000000000 ) ) ;
#2903 = CARTESIAN_POINT ( 'NONE',  ( -32.32195836398363298, 75.59155356138302295, 7.099754829268524858 ) ) ;
#2904 = FACE_OUTER_BOUND ( 'NONE', #5361, .T. ) ;
#2905 = VECTOR ( 'NONE', #9384, 1000.000000000000000 ) ;
#2906 = EDGE_CURVE ( 'NONE', #10814, #5994, #9098, .T. ) ;
#2907 = DIRECTION ( 'NONE',  ( 0.000000000000000000, 0.000000000000000000, 1.000000000000000000 ) ) ;
#2908 = B_SPLINE_CURVE_WITH_KNOTS ( 'NONE', 3,
 ( #9291, #12303, #9411, #4565, #3, #11426, #2820, #11180, #1763, #1824, #12122, #3571, #7500, #6622, #1706, #12185, #892, #7618, #11246, #9350, #4750, #10417, #2695, #3818, #6507, #1880 ),
 .UNSPECIFIED., .F., .F.,
 ( 4, 2, 2, 2, 2, 2, 2, 2, 2, 2, 2, 2, 4 ),
 ( 1.040834085586084257E-17, 0.001946127227419483172, 0.002919190841129219553, 0.003892254454838955935, 0.005838381682258432168, 0.006811445295968166815, 0.007784508909677901461, 0.008757572523387635241, 0.009730636137097370755, 0.01167676336451683311, 0.01264982697822655995, 0.01362289059193628506, 0.01556901781935573353 ),
 .UNSPECIFIED. ) ;
#2909 = CARTESIAN_POINT ( 'NONE',  ( 70.92179708824016870, 47.98984913414685849, -24.39594572817711438 ) ) ;
#2910 = VECTOR ( 'NONE', #4647, 1000.000000000000000 ) ;
#2911 = DIRECTION ( 'NONE',  ( 1.000000000000000000, -1.040834085586083310E-14, 0.000000000000000000 ) ) ;
#2912 = CARTESIAN_POINT ( 'NONE',  ( -5.999999999999999112, 62.00000000000000000, 60.00000000000002132 ) ) ;
#2913 =( BOUNDED_CURVE ( )  B_SPLINE_CURVE ( 2, ( #8119, #6202, #9994, #4448, #8246 ),
 .UNSPECIFIED., .F., .F. ) 
 B_SPLINE_CURVE_WITH_KNOTS ( ( 3, 2, 3 ),
 ( 0.9375000000000007772, 0.9687500000000004441, 1.000000000000000000 ),
 .UNSPECIFIED. ) 
 CURVE ( )  GEOMETRIC_REPRESENTATION_ITEM ( )  RATIONAL_B_SPLINE_CURVE ( ( 0.9999999999999981126, 0.9238795325112886259, 1.000000000000000000, 0.9238795325112867385, 1.000000000000000000 ) ) 
 REPRESENTATION_ITEM ( '' )  );
#2914 = DIRECTION ( 'NONE',  ( 0.4999999999999985012, -0.8660254037844394848, 0.000000000000000000 ) ) ;
#2915 = ADVANCED_FACE ( 'NONE', ( #10085 ), #11031, .T. ) ;
#2916 = DIRECTION ( 'NONE',  ( 0.000000000000000000, 1.000000000000000000, 0.000000000000000000 ) ) ;
#2917 = LINE ( 'NONE', #5847, #11473 ) ;
#2918 = ORIENTED_EDGE ( 'NONE', *, *, #4353, .T. ) ;
#2919 = PRODUCT_RELATED_PRODUCT_CATEGORY ( 'part', '', ( #10458 ) ) ;
#2920 = EDGE_CURVE ( 'NONE', #8405, #4965, #4486, .T. ) ;
#2921 = CARTESIAN_POINT ( 'NONE',  ( 8.572527594031474570E-15, 5.000000000000129674, -70.00000000000001421 ) ) ;
#2922 = CARTESIAN_POINT ( 'NONE',  ( 0.000000000000000000, 115.0000000000000000, 0.000000000000000000 ) ) ;
#2923 = EDGE_LOOP ( 'NONE', ( #12285, #10145 ) ) ;
#2924 = DIRECTION ( 'NONE',  ( 0.000000000000000000, 0.000000000000000000, 1.000000000000000000 ) ) ;
#2925 = AXIS2_PLACEMENT_3D ( 'NONE', #6751, #8546, #1146 ) ;
#2926 = VERTEX_POINT ( 'NONE', #12040 ) ;
#2927 = DIRECTION ( 'NONE',  ( 0.000000000000000000, 1.000000000000000000, 0.000000000000000000 ) ) ;
#2928 = CARTESIAN_POINT ( 'NONE',  ( 74.16198487095664404, 40.36295898505520086, 25.00000000000000355 ) ) ;
#2929 = EDGE_LOOP ( 'NONE', ( #328, #7017, #787 ) ) ;
#2930 = VECTOR ( 'NONE', #10980, 1000.000000000000000 ) ;
#2931 = LINE ( 'NONE', #3988, #5877 ) ;
#2932 = EDGE_CURVE ( 'NONE', #8296, #7815, #1162, .T. ) ;
#2933 = CARTESIAN_POINT ( 'NONE',  ( 0.000000000000000000, 165.0000000000000000, 2.099999999999988987 ) ) ;
#2934 = ORIENTED_EDGE ( 'NONE', *, *, #354, .T. ) ;
#2935 = PRODUCT_CONTEXT ( 'NONE', #10591, 'mechanical' ) ;
#2936 = CARTESIAN_POINT ( 'NONE',  ( 145.0000000000011369, 225.0000000000000853, -25.00000000000000000 ) ) ;
#2937 = DIRECTION ( 'NONE',  ( -0.7236679289129753778, 0.000000000000000000, 0.6901483381584025967 ) ) ;
#2938 = CARTESIAN_POINT ( 'NONE',  ( 2.500000000000000000, 2.357898499370431722, -2.818925648462311528E-15 ) ) ;
#2939 = EDGE_LOOP ( 'NONE', ( #12230, #8447, #10864, #2891 ) ) ;
#2940 = CARTESIAN_POINT ( 'NONE',  ( 1.121994411437819528, 114.1249999986344079, -2.708734124999999882 ) ) ;
#2941 = CARTESIAN_POINT ( 'NONE',  ( -1.346194077712560944, 111.5624999972688300, -3.249999999999999556 ) ) ;
#2942 = ORIENTED_EDGE ( 'NONE', *, *, #3703, .F. ) ;
#2943 = CARTESIAN_POINT ( 'NONE',  ( -24.99999999999999289, 450.0000000000000568, -14.99999999999999289 ) ) ;
#2944 = CARTESIAN_POINT ( 'NONE',  ( 150.0000000000010800, 15.00000000000008882, -19.99999999999999645 ) ) ;
#2945 = EDGE_LOOP ( 'NONE', ( #8906, #6831, #3725, #818 ) ) ;
#2946 = CYLINDRICAL_SURFACE ( 'NONE', #831, 5.000000000000000888 ) ;
#2947 = DIRECTION ( 'NONE',  ( -3.469446951953613696E-16, 0.000000000000000000, 1.000000000000000000 ) ) ;
#2948 = ORIENTED_EDGE ( 'NONE', *, *, #4601, .T. ) ;
#2949 = CARTESIAN_POINT ( 'NONE',  ( -1.440781129305261477, 20.00000000000009592, 79.50000000000000000 ) ) ;
#2950 = PLANE ( 'NONE',  #11697 ) ;
#2951 = PLANE ( 'NONE',  #5593 ) ;
#2952 = EDGE_CURVE ( 'NONE', #9665, #9381, #2555, .T. ) ;
#2953 = LINE ( 'NONE', #5706, #10753 ) ;
#2954 = CARTESIAN_POINT ( 'NONE',  ( 1.346194077712559833, 110.8124999999999858, -3.250000000000000000 ) ) ;
#2955 = EDGE_CURVE ( 'NONE', #8153, #2768, #8281, .T. ) ;
#2956 = CARTESIAN_POINT ( 'NONE',  ( -2.708734124999999882, 111.9999999986343937, 1.121994411437819084 ) ) ;
#2957 = SHAPE_REPRESENTATION_RELATIONSHIP ( 'NONE' , 'NONE' ,  #8876, #6166 ) ;
#2958 = VECTOR ( 'NONE', #3371, 1000.000000000000000 ) ;
#2959 = ORIENTED_EDGE ( 'NONE', *, *, #365, .F. ) ;
#2960 = DIRECTION ( 'NONE',  ( 0.000000000000000000, 0.000000000000000000, -1.000000000000000000 ) ) ;
#2961 = CARTESIAN_POINT ( 'NONE',  ( 13.72352623184575293, 31.85795502388325673, 73.73395739868169585 ) ) ;
#2962 = EDGE_LOOP ( 'NONE', ( #76, #10415 ) ) ;
#2963 = DIRECTION ( 'NONE',  ( 0.000000000000000000, 0.000000000000000000, 1.000000000000000000 ) ) ;
#2964 = PRESENTATION_STYLE_ASSIGNMENT (( #4902 ) ) ;
#2965 = EDGE_CURVE ( 'NONE', #2816, #1278, #6337, .T. ) ;
#2966 = AXIS2_PLACEMENT_3D ( 'NONE', #9399, #4429, #10155 ) ;
#2967 = ORIENTED_EDGE ( 'NONE', *, *, #10354, .T. ) ;
#2968 = ORIENTED_EDGE ( 'NONE', *, *, #2806, .F. ) ;
#2969 = SURFACE_STYLE_FILL_AREA ( #9685 ) ;
#2970 = EDGE_CURVE ( 'NONE', #3368, #6910, #556, .T. ) ;
#2971 = ORIENTED_EDGE ( 'NONE', *, *, #5540, .T. ) ;
#2972 = CARTESIAN_POINT ( 'NONE',  ( 70.44139041661959766, 46.67990480737745429, -25.75312943552223288 ) ) ;
#2973 = PLANE ( 'NONE',  #3776 ) ;
#2974 = EDGE_CURVE ( 'NONE', #8555, #7080, #10511, .T. ) ;
#2975 = EDGE_CURVE ( 'NONE', #11714, #7098, #7526, .T. ) ;
#2976 = DIRECTION ( 'NONE',  ( -0.8660254037844398178, -0.4999999999999977796, 0.000000000000000000 ) ) ;
#2977 = LINE ( 'NONE', #10576, #8961 ) ;
#2978 = CARTESIAN_POINT ( 'NONE',  ( 77.45966692414835109, 15.00000000000009059, -19.99999999999999645 ) ) ;
#2979 = ORIENTED_EDGE ( 'NONE', *, *, #9192, .F. ) ;
#2980 = CARTESIAN_POINT ( 'NONE',  ( -32.14616437604218646, 85.84037417286381810, -9.329764321300741514 ) ) ;
#2981 = CARTESIAN_POINT ( 'NONE',  ( 0.000000000000000000, 165.0000000000000000, 0.000000000000000000 ) ) ;
#2982 = AXIS2_PLACEMENT_3D ( 'NONE', #10327, #6353, #9325 ) ;
#2983 = VECTOR ( 'NONE', #5875, 1000.000000000000000 ) ;
#2984 = EDGE_LOOP ( 'NONE', ( #1803, #9733, #9734, #886 ) ) ;
#2985 = CYLINDRICAL_SURFACE ( 'NONE', #2004, 35.00000000000000711 ) ;
#2986 = ORIENTED_EDGE ( 'NONE', *, *, #3568, .T. ) ;
#2987 = DIRECTION ( 'NONE',  ( 0.8660254037844408170, -0.4999999999999961697, 0.000000000000000000 ) ) ;
#2988 = VECTOR ( 'NONE', #703, 1000.000000000000000 ) ;
#2989 = CARTESIAN_POINT ( 'NONE',  ( 75.52936542331360670, 43.86594787320247235, 23.18670291617644352 ) ) ;
#2990 = EDGE_LOOP ( 'NONE', ( #1104, #11477 ) ) ;
#2991 = DIRECTION ( 'NONE',  ( 0.000000000000000000, 1.000000000000000000, 0.000000000000000000 ) ) ;
#2992 = DIRECTION ( 'NONE',  ( 0.8660254037844331565, -0.5000000000000095479, 0.000000000000000000 ) ) ;
#2993 = VERTEX_POINT ( 'NONE', #5675 ) ;
#2994 = APPLICATION_PROTOCOL_DEFINITION ( 'draft international standard', 'automotive_design', 1998, #10591 ) ;
#2995 = DIRECTION ( 'NONE',  ( 0.5000000000000001110, 0.8660254037844387076, 0.000000000000000000 ) ) ;
#2996 = DIRECTION ( 'NONE',  ( -0.4999999999999942268, 0.8660254037844419273, 0.000000000000000000 ) ) ;
#2997 = ORIENTED_EDGE ( 'NONE', *, *, #1441, .F. ) ;
#2998 = CARTESIAN_POINT ( 'NONE',  ( -4.975863863883684959E-16, 112.0624999986344079, -2.708734125000000326 ) ) ;
#2999 = CARTESIAN_POINT ( 'NONE',  ( -3.250000000000000444, 113.3749999972688158, 3.980102097228898231E-16 ) ) ;
#3000 = AXIS2_PLACEMENT_3D ( 'NONE', #5270, #9049, #8056 ) ;
#3001 = EDGE_CURVE ( 'NONE', #11680, #10543, #9583, .T. ) ;
#3002 = VERTEX_POINT ( 'NONE', #109 ) ;
#3003 = DIRECTION ( 'NONE',  ( -0.000000000000000000, 1.000000000000000000, -0.000000000000000000 ) ) ;
#3004 = EDGE_CURVE ( 'NONE', #8712, #8042, #1862, .T. ) ;
#3005 = DIRECTION ( 'NONE',  ( 0.000000000000000000, 1.000000000000000000, 0.000000000000000000 ) ) ;
#3006 = VERTEX_POINT ( 'NONE', #999 ) ;
#3007 = CARTESIAN_POINT ( 'NONE',  ( 5.200000000000002842, 0.000000000000000000, 2.500000000000000444 ) ) ;
#3008 = DIRECTION ( 'NONE',  ( -0.9682458365518543664, 0.000000000000000000, -0.2499999999999996947 ) ) ;
#3009 = CONICAL_SURFACE ( 'NONE', #11962, 2.055000000000000160, 0.7853981633974639331 ) ;
#3010 = CIRCLE ( 'NONE', #7779, 3.250000000000000444 ) ;
#3011 = VERTEX_POINT ( 'NONE', #2860 ) ;
#3012 = CARTESIAN_POINT ( 'NONE',  ( -14.19078112930533209, 29.75000000000008882, 79.50000000000000000 ) ) ;
#3013 = CARTESIAN_POINT ( 'NONE',  ( 5.092712519748452848, 41.38333024919784719, 79.50000000000000000 ) ) ;
#3014 = DIRECTION ( 'NONE',  ( -1.000000000000000000, 0.000000000000000000, 0.000000000000000000 ) ) ;
#3015 = CARTESIAN_POINT ( 'NONE',  ( -1.190781129305471087, 30.00000000000008882, 80.00000000000000000 ) ) ;
#3016 = PLANE ( 'NONE',  #7168 ) ;
#3017 = CIRCLE ( 'NONE', #9773, 2.099999999999988987 ) ;
#3018 = CARTESIAN_POINT ( 'NONE',  ( -1.915364268218909594, 112.1874999986344079, -1.915364268218908927 ) ) ;
#3019 = ORIENTED_EDGE ( 'NONE', *, *, #3568, .F. ) ;
#3020 = ORIENTED_EDGE ( 'NONE', *, *, #12206, .T. ) ;
#3021 = DIRECTION ( 'NONE',  ( 0.000000000000000000, -1.000000000000000000, -0.000000000000000000 ) ) ;
#3022 = CARTESIAN_POINT ( 'NONE',  ( 25.00000000000000000, 445.0000000000000568, -59.99999999999999289 ) ) ;
#3023 = ORIENTED_EDGE ( 'NONE', *, *, #7075, .T. ) ;
#3024 = VECTOR ( 'NONE', #4583, 1000.000000000000000 ) ;
#3025 = CARTESIAN_POINT ( 'NONE',  ( 0.000000000000000000, 165.5000000000000000, 2.649999999999993694 ) ) ;
#3026 = CARTESIAN_POINT ( 'NONE',  ( 109.9268209223821628, 275.0000000000000000, 32.26598893414752212 ) ) ;
#3027 = CIRCLE ( 'NONE', #4215, 4.999999999999998224 ) ;
#3028 = LINE ( 'NONE', #9682, #8873 ) ;
#3029 = PLANE ( 'NONE',  #10359 ) ;
#3030 = ORIENTED_EDGE ( 'NONE', *, *, #408, .F. ) ;
#3031 = ORIENTED_EDGE ( 'NONE', *, *, #4877, .F. ) ;
#3032 = DIRECTION ( 'NONE',  ( 0.000000000000000000, 0.000000000000000000, 1.000000000000000000 ) ) ;
#3033 = ORIENTED_EDGE ( 'NONE', *, *, #6455, .T. ) ;
#3034 = EDGE_CURVE ( 'NONE', #2993, #9781, #9458, .T. ) ;
#3035 = CARTESIAN_POINT ( 'NONE',  ( 0.000000000000000000, 92.00000000000000000, 24.99999999999999645 ) ) ;
#3036 = DIRECTION ( 'NONE',  ( 0.000000000000000000, 1.000000000000000000, 0.000000000000000000 ) ) ;
#3037 = CARTESIAN_POINT ( 'NONE',  ( 2.298097038856279806, 113.1250000000000000, 2.298097038856279806 ) ) ;
#3038 = CARTESIAN_POINT ( 'NONE',  ( 75.38891993288051196, 16.31599220047735344, -23.38442328187116104 ) ) ;
#3039 = VERTEX_POINT ( 'NONE', #4669 ) ;
#3040 = DIRECTION ( 'NONE',  ( 0.000000000000000000, -1.000000000000000000, 1.287488025362403787E-15 ) ) ;
#3041 = DIRECTION ( 'NONE',  ( 0.000000000000000000, -1.000000000000000000, 0.000000000000000000 ) ) ;
#3042 = AXIS2_PLACEMENT_3D ( 'NONE', #7697, #913, #6827 ) ;
#3043 = ORIENTED_EDGE ( 'NONE', *, *, #6726, .F. ) ;
#3044 = CARTESIAN_POINT ( 'NONE',  ( 0.000000000000000000, 109.0000000000000000, 0.000000000000000000 ) ) ;
#3045 = EDGE_CURVE ( 'NONE', #1500, #12351, #939, .T. ) ;
#3046 = EDGE_CURVE ( 'NONE', #4833, #10602, #4728, .T. ) ;
#3047 = ORIENTED_EDGE ( 'NONE', *, *, #8065, .T. ) ;
#3048 = TOROIDAL_SURFACE ( 'NONE', #11820, 24.99999999999999645, 0.5000000000000004441 ) ;
#3049 = LINE ( 'NONE', #10467, #6934 ) ;
#3050 = DIRECTION ( 'NONE',  ( -0.9717889794219070065, 0.000000000000000000, -0.2358520287683117111 ) ) ;
#3051 = ORIENTED_EDGE ( 'NONE', *, *, #200, .F. ) ;
#3052 = CARTESIAN_POINT ( 'NONE',  ( 0.000000000000000000, 110.0000000000000000, 0.000000000000000000 ) ) ;
#3053 = DIRECTION ( 'NONE',  ( 0.000000000000000000, 0.000000000000000000, -1.000000000000000000 ) ) ;
#3054 = ORIENTED_EDGE ( 'NONE', *, *, #4953, .F. ) ;
#3055 = SHAPE_DEFINITION_REPRESENTATION ( #6681, #7136 ) ;
#3056 = DIRECTION ( 'NONE',  ( 0.000000000000000000, -1.000000000000000000, -0.000000000000000000 ) ) ;
#3057 = EDGE_CURVE ( 'NONE', #12307, #9534, #3049, .T. ) ;
#3058 = CARTESIAN_POINT ( 'NONE',  ( -5.974274778359173865, 21.21474596215567487, 79.50000000000000000 ) ) ;
#3059 = ORIENTED_EDGE ( 'NONE', *, *, #681, .T. ) ;
#3060 = CARTESIAN_POINT ( 'NONE',  ( 149.1421356237320026, 17.07106781186555722, 24.99999999999999645 ) ) ;
#3061 = AXIS2_PLACEMENT_3D ( 'NONE', #8815, #7143, #6091 ) ;
#3062 = CARTESIAN_POINT ( 'NONE',  ( 2.298097038856279806, 111.9999999972688158, 2.298097038856279806 ) ) ;
#3063 = ORIENTED_EDGE ( 'NONE', *, *, #3034, .F. ) ;
#3064 = DIRECTION ( 'NONE',  ( 0.000000000000000000, 0.000000000000000000, -1.000000000000000000 ) ) ;
#3065 = LINE ( 'NONE', #6745, #9242 ) ;
#3066 = EDGE_LOOP ( 'NONE', ( #1337, #8361, #7237, #7200 ) ) ;
#3067 = LINE ( 'NONE', #11733, #1226 ) ;
#3068 = PLANE ( 'NONE',  #11071 ) ;
#3069 = EDGE_LOOP ( 'NONE', ( #8765, #5742, #9232, #10691 ) ) ;
#3070 = VECTOR ( 'NONE', #5085, 1000.000000000000000 ) ;
#3071 = DIRECTION ( 'NONE',  ( -0.000000000000000000, -1.000000000000000000, -0.000000000000000000 ) ) ;
#3072 = EDGE_CURVE ( 'NONE', #11346, #3399, #3927, .T. ) ;
#3073 = EDGE_CURVE ( 'NONE', #10304, #11439, #7914, .T. ) ;
#3074 = FACE_OUTER_BOUND ( 'NONE', #426, .T. ) ;
#3075 = CARTESIAN_POINT ( 'NONE',  ( 0.000000000000000000, -2.357898499370432166, 3.035766082959412415E-15 ) ) ;
#3076 = CARTESIAN_POINT ( 'NONE',  ( 2.708734124999999882, 114.5624999986344079, 0.000000000000000000 ) ) ;
#3077 = CARTESIAN_POINT ( 'NONE',  ( -7.907287480251413925, 18.86666975080236597, 79.50000000000000000 ) ) ;
#3078 = CARTESIAN_POINT ( 'NONE',  ( -1.915364268218908927, 113.9374999986344079, 1.915364268218909150 ) ) ;
#3079 = CONICAL_SURFACE ( 'NONE', #685, 2.099999999999998312, 1.029744258676656532 ) ;
#3080 = EDGE_LOOP ( 'NONE', ( #9286, #4717, #12223, #3130 ) ) ;
#3081 = ORIENTED_EDGE ( 'NONE', *, *, #2310, .F. ) ;
#3082 = LINE ( 'NONE', #8866, #8432 ) ;
#3083 = DIRECTION ( 'NONE',  ( -0.000000000000000000, -0.000000000000000000, -1.000000000000000000 ) ) ;
#3084 = ORIENTED_EDGE ( 'NONE', *, *, #2158, .T. ) ;
#3085 = CARTESIAN_POINT ( 'NONE',  ( -89.80805993797480369, 285.0000000000000568, 71.82974571984181011 ) ) ;
#3086 = CARTESIAN_POINT ( 'NONE',  ( 5.200000000000002842, 0.000000000000000000, 0.000000000000000000 ) ) ;
#3087 = SURFACE_STYLE_FILL_AREA ( #5899 ) ;
#3088 = CYLINDRICAL_SURFACE ( 'NONE', #216, 73.00000000000002842 ) ;
#3089 = TOROIDAL_SURFACE ( 'NONE', #9039, 10.00000000000000000, 5.000000000000000000 ) ;
#3090 = TOROIDAL_SURFACE ( 'NONE', #7477, 17.00000000000000000, 0.5000000000000004441 ) ;
#3091 = ORIENTED_EDGE ( 'NONE', *, *, #9038, .F. ) ;
#3092 = VERTEX_POINT ( 'NONE', #10399 ) ;
#3093 = VECTOR ( 'NONE', #6841, 1000.000000000000000 ) ;
#3094 = DIRECTION ( 'NONE',  ( 0.8660254037844399289, 0.4999999999999977796, 0.000000000000000000 ) ) ;
#3095 = DIRECTION ( 'NONE',  ( 1.000000000000000000, 0.000000000000000000, 0.000000000000000000 ) ) ;
#3096 = ORIENTED_EDGE ( 'NONE', *, *, #4197, .F. ) ;
#3097 =( NAMED_UNIT ( * ) PLANE_ANGLE_UNIT ( ) SI_UNIT ( $, .RADIAN. ) );
#3098 = PLANE ( 'NONE',  #11873 ) ;
#3099 = ADVANCED_FACE ( 'NONE', ( #5736 ), #6791, .T. ) ;
#3100 = CYLINDRICAL_SURFACE ( 'NONE', #9425, 15.00000000000000000 ) ;
#3101 = B_SPLINE_CURVE_WITH_KNOTS ( 'NONE', 3,
 ( #2151, #9741, #6708, #5958 ),
 .UNSPECIFIED., .F., .F.,
 ( 4, 4 ),
 ( 0.0002502309401076680852, 0.0005002309401076784987 ),
 .UNSPECIFIED. ) ;
#3102 = CARTESIAN_POINT ( 'NONE',  ( 0.000000000000000000, 65.00000000000000000, 0.000000000000000000 ) ) ;
#3103 = EDGE_CURVE ( 'NONE', #11846, #1468, #171, .T. ) ;
#3104 = CIRCLE ( 'NONE', #4504, 35.00000000000000000 ) ;
#3105 = ORIENTED_EDGE ( 'NONE', *, *, #11826, .F. ) ;
#3106 = CYLINDRICAL_SURFACE ( 'NONE', #813, 30.00000000000000000 ) ;
#3107 = EDGE_CURVE ( 'NONE', #2738, #8492, #3798, .T. ) ;
#3108 = CIRCLE ( 'NONE', #725, 9.999999999999998224 ) ;
#3109 = ORIENTED_EDGE ( 'NONE', *, *, #2496, .T. ) ;
#3110 = CARTESIAN_POINT ( 'NONE',  ( -73.35315233757310693, 81.28571428571424917, 1.237179148263527928 ) ) ;
#3111 = CARTESIAN_POINT ( 'NONE',  ( 9.942549119892413856, 23.28349364905404428, 79.50000000000000000 ) ) ;
#3112 = ORIENTED_EDGE ( 'NONE', *, *, #3965, .T. ) ;
#3113 = DIRECTION ( 'NONE',  ( 1.000000000000000000, -0.000000000000000000, 1.224646799147353207E-16 ) ) ;
#3114 = CARTESIAN_POINT ( 'NONE',  ( -5.970153145843347347E-16, 111.6249999972688158, -3.250000000000000444 ) ) ;
#3115 = ORIENTED_EDGE ( 'NONE', *, *, #8011, .F. ) ;
#3116 = LINE ( 'NONE', #1064, #12055 ) ;
#3117 = VECTOR ( 'NONE', #6095, 1000.000000000000114 ) ;
#3118 = DIRECTION ( 'NONE',  ( 0.000000000000000000, 0.000000000000000000, 1.000000000000000000 ) ) ;
#3119 = EDGE_CURVE ( 'NONE', #11350, #8283, #876, .T. ) ;
#3120 = ORIENTED_EDGE ( 'NONE', *, *, #6635, .T. ) ;
#3121 = CARTESIAN_POINT ( 'NONE',  ( -1.121994411437820416, 111.9999999986343937, -2.708734124999999882 ) ) ;
#3122 = CARTESIAN_POINT ( 'NONE',  ( 2.298097038856279806, 113.9999999972688158, 2.298097038856279806 ) ) ;
#3123 = AXIS2_PLACEMENT_3D ( 'NONE', #8484, #6815, #10612 ) ;
#3124 = ORIENTED_EDGE ( 'NONE', *, *, #2648, .F. ) ;
#3125 = DIRECTION ( 'NONE',  ( -0.000000000000000000, -0.000000000000000000, 1.000000000000000000 ) ) ;
#3126 = CARTESIAN_POINT ( 'NONE',  ( 0.000000000000000000, 127.0000000000000000, -17.50000000000000000 ) ) ;
#3127 = ORIENTED_EDGE ( 'NONE', *, *, #1396, .F. ) ;
#3128 = FACE_OUTER_BOUND ( 'NONE', #7169, .T. ) ;
#3129 = CARTESIAN_POINT ( 'NONE',  ( 21.00000000000000355, 0.000000000000000000, 2.055000000000000160 ) ) ;
#3130 = ORIENTED_EDGE ( 'NONE', *, *, #775, .T. ) ;
#3131 = EDGE_CURVE ( 'NONE', #7450, #7160, #6738, .T. ) ;
#3132 = ADVANCED_FACE ( 'NONE', ( #9517 ), #8462, .T. ) ;
#3133 = DIRECTION ( 'NONE',  ( 0.000000000000000000, -0.8660254037844401509, 0.4999999999999974465 ) ) ;
#3134 = CARTESIAN_POINT ( 'NONE',  ( -27.30107202361637775, 86.87046582918780757, -12.43589427268144831 ) ) ;
#3135 = CARTESIAN_POINT ( 'NONE',  ( -34.84121487603211875, 75.26794919243111792, 7.660254037844449471 ) ) ;
#3136 = ORIENTED_EDGE ( 'NONE', *, *, #9839, .F. ) ;
#3137 = CARTESIAN_POINT ( 'NONE',  ( 3.517098443892134441, 31.48290155610792596, 57.08203932499370836 ) ) ;
#3138 = CARTESIAN_POINT ( 'NONE',  ( -1.121994411437820194, 114.2499999986344079, -2.708734124999999437 ) ) ;
#3139 = EDGE_LOOP ( 'NONE', ( #10165, #8832, #1684, #4816 ) ) ;
#3140 = VERTEX_POINT ( 'NONE', #4795 ) ;
#3141 = EDGE_CURVE ( 'NONE', #9412, #3881, #12286, .T. ) ;
#3142 = PRODUCT_DEFINITION_CONTEXT ( 'detailed design', #397, 'design' ) ;
#3143 = LINE ( 'NONE', #8684, #2662 ) ;
#3144 = DIRECTION ( 'NONE',  ( 0.000000000000000000, 0.000000000000000000, 1.000000000000000000 ) ) ;
#3145 = ORIENTED_EDGE ( 'NONE', *, *, #6573, .F. ) ;
#3146 = CARTESIAN_POINT ( 'NONE',  ( 0.000000000000000000, 165.0000000000000000, 0.000000000000000000 ) ) ;
#3147 = CARTESIAN_POINT ( 'NONE',  ( 0.000000000000000000, 0.000000000000000000, 25.00000000000000000 ) ) ;
#3148 = DIRECTION ( 'NONE',  ( 0.5000000000000038858, 0.8660254037844363761, 0.000000000000000000 ) ) ;
#3149 = LINE ( 'NONE', #2272, #12173 ) ;
#3150 = AXIS2_PLACEMENT_3D ( 'NONE', #3615, #2497, #5555 ) ;
#3151 =( GEOMETRIC_REPRESENTATION_CONTEXT ( 3 ) GLOBAL_UNCERTAINTY_ASSIGNED_CONTEXT ( ( #2779 ) ) GLOBAL_UNIT_ASSIGNED_CONTEXT ( ( #12007, #5397, #3462 ) ) REPRESENTATION_CONTEXT ( 'NONE', 'WORKASPACE' ) );
#3152 = ORIENTED_EDGE ( 'NONE', *, *, #11598, .T. ) ;
#3153 = ORIENTED_EDGE ( 'NONE', *, *, #2932, .F. ) ;
#3154 = EDGE_CURVE ( 'NONE', #3039, #3929, #7659, .T. ) ;
#3155 = DIRECTION ( 'NONE',  ( -0.000000000000000000, -1.000000000000000000, -0.000000000000000000 ) ) ;
#3156 = VECTOR ( 'NONE', #5587, 1000.000000000000000 ) ;
#3157 = CARTESIAN_POINT ( 'NONE',  ( -1.190781129305471087, 30.00000000000008882, 80.00000000000000000 ) ) ;
#3158 = DIRECTION ( 'NONE',  ( 0.000000000000000000, 1.000000000000000000, 0.000000000000000000 ) ) ;
#3159 = CARTESIAN_POINT ( 'NONE',  ( 70.75727862648629696, 12.41690240222903618, -24.86906317558853274 ) ) ;
#3160 = FACE_OUTER_BOUND ( 'NONE', #10147, .T. ) ;
#3161 = CARTESIAN_POINT ( 'NONE',  ( 1.658621287961228566E-16, 112.5624999986344079, 2.708734125000000326 ) ) ;
#3162 = EDGE_LOOP ( 'NONE', ( #2022, #11244, #6013, #9011, #11184 ) ) ;
#3163 = CARTESIAN_POINT ( 'NONE',  ( 4.999999999999997335, 5.204748896376250699E-16, -4.250000000000000000 ) ) ;
#3164 = EDGE_CURVE ( 'NONE', #5158, #2274, #46, .T. ) ;
#3165 = EDGE_LOOP ( 'NONE', ( #9598, #8663, #9347, #10099, #10565 ) ) ;
#3166 = CARTESIAN_POINT ( 'NONE',  ( -12.57411137850303540, 36.28349364905398033, 79.50000000000000000 ) ) ;
#3167 = PRESENTATION_LAYER_ASSIGNMENT (  '', '', ( #7865 ) ) ;
#3168 = ORIENTED_EDGE ( 'NONE', *, *, #1176, .T. ) ;
#3169 = EDGE_CURVE ( 'NONE', #9835, #8030, #1056, .T. ) ;
#3170 = CARTESIAN_POINT ( 'NONE',  ( 0.000000000000000000, 345.0000000000000568, 0.000000000000000000 ) ) ;
#3171 = CARTESIAN_POINT ( 'NONE',  ( 0.000000000000000000, 52.00000000000000711, 0.000000000000000000 ) ) ;
#3172 = ORIENTED_EDGE ( 'NONE', *, *, #3344, .F. ) ;
#3173 = CIRCLE ( 'NONE', #5775, 15.00000000000000000 ) ;
#3174 = AXIS2_PLACEMENT_3D ( 'NONE', #127, #2818, #7616 ) ;
#3175 = DIRECTION ( 'NONE',  ( -0.000000000000000000, -0.000000000000000000, 1.000000000000000000 ) ) ;
#3176 =( GEOMETRIC_REPRESENTATION_CONTEXT ( 3 ) GLOBAL_UNCERTAINTY_ASSIGNED_CONTEXT ( ( #10383 ) ) GLOBAL_UNIT_ASSIGNED_CONTEXT ( ( #463, #2462, #11701 ) ) REPRESENTATION_CONTEXT ( 'NONE', 'WORKASPACE' ) );
#3177 = CARTESIAN_POINT ( 'NONE',  ( -29.14112381217239900, 87.50172632198250255, -9.529269519012833811 ) ) ;
#3178 = VERTEX_POINT ( 'NONE', #11073 ) ;
#3179 = CARTESIAN_POINT ( 'NONE',  ( 2.708734125000000326, 113.3749999986344079, 1.121994411437818862 ) ) ;
#3180 = CIRCLE ( 'NONE', #9739, 0.5000000000000004441 ) ;
#3181 = APPLICATION_CONTEXT ( 'automotive_design' ) ;
#3182 = ORIENTED_EDGE ( 'NONE', *, *, #11643, .F. ) ;
#3183 = CIRCLE ( 'NONE', #4373, 10.00000000000000178 ) ;
#3184 = EDGE_CURVE ( 'NONE', #3370, #3011, #4328, .T. ) ;
#3185 = ADVANCED_FACE ( 'NONE', ( #1594 ), #6914, .F. ) ;
#3186 = CARTESIAN_POINT ( 'NONE',  ( 27.88763417807735578, 88.17431669512683357, 10.69423021798056084 ) ) ;
#3187 = DIRECTION ( 'NONE',  ( 0.000000000000000000, 0.000000000000000000, 1.000000000000000000 ) ) ;
#3188 = EDGE_LOOP ( 'NONE', ( #2326, #2231, #8721, #9253, #1704, #11944 ) ) ;
#3189 = CIRCLE ( 'NONE', #5978, 5.000000000000000888 ) ;
#3190 = CARTESIAN_POINT ( 'NONE',  ( -0.9407811293052825707, 17.00000000000008882, 80.00000000000000000 ) ) ;
#3191 = LINE ( 'NONE', #9029, #12268 ) ;
#3192 = EDGE_LOOP ( 'NONE', ( #8165, #4054, #9076, #504 ) ) ;
#3193 = DIRECTION ( 'NONE',  ( 0.000000000000000000, 0.000000000000000000, -1.000000000000000000 ) ) ;
#3194 = CARTESIAN_POINT ( 'NONE',  ( 76.05876219242703939, 44.39552472664445304, -22.40335076292606331 ) ) ;
#3195 = DIRECTION ( 'NONE',  ( -0.000000000000000000, -1.000000000000000000, -0.000000000000000000 ) ) ;
#3196 = AXIS2_PLACEMENT_3D ( 'NONE', #7951, #3289, #9823 ) ;
#3197 = VERTEX_POINT ( 'NONE', #8067 ) ;
#3198 = CARTESIAN_POINT ( 'NONE',  ( -7.690781129305409358, 41.25833024919774772, 80.00000000000000000 ) ) ;
#3199 = CARTESIAN_POINT ( 'NONE',  ( 76.56943592554333122, 15.25648089810431429, 21.58906638518815768 ) ) ;
#3200 = EDGE_CURVE ( 'NONE', #3448, #9390, #7142, .T. ) ;
#3201 = VECTOR ( 'NONE', #721, 1000.000000000000000 ) ;
#3202 = ORIENTED_EDGE ( 'NONE', *, *, #10324, .F. ) ;
#3203 = CARTESIAN_POINT ( 'NONE',  ( 75.04559065614574820, 16.80434123660322143, 23.85935468423092587 ) ) ;
#3204 = CARTESIAN_POINT ( 'NONE',  ( 72.13972991039015881, 45.12505515914934051, -20.57104709750046467 ) ) ;
#3205 = VERTEX_POINT ( 'NONE', #11891 ) ;
#3206 = LINE ( 'NONE', #7008, #9424 ) ;
#3207 = CARTESIAN_POINT ( 'NONE',  ( 70.52159520668648440, 46.91448669815612504, 25.52954545350316451 ) ) ;
#3208 = VERTEX_POINT ( 'NONE', #11659 ) ;
#3209 = DIRECTION ( 'NONE',  ( -0.000000000000000000, -0.000000000000000000, 1.000000000000000000 ) ) ;
#3210 = PLANE ( 'NONE',  #10957 ) ;
#3211 = DIRECTION ( 'NONE',  ( 0.000000000000000000, 0.000000000000000000, 1.000000000000000000 ) ) ;
#3212 = CARTESIAN_POINT ( 'NONE',  ( -1.121994411437819084, 110.6249999986343937, 2.708734125000000326 ) ) ;
#3213 = EDGE_CURVE ( 'NONE', #9112, #1030, #9313, .T. ) ;
#3214 = CIRCLE ( 'NONE', #7400, 25.50000000000000000 ) ;
#3215 = PRESENTATION_STYLE_ASSIGNMENT (( #2217 ) ) ;
#3216 = VERTEX_POINT ( 'NONE', #1183 ) ;
#3217 = AXIS2_PLACEMENT_3D ( 'NONE', #11462, #6429, #12168 ) ;
#3218 =( BOUNDED_SURFACE ( )  B_SPLINE_SURFACE ( 3, 2, ( 
 ( #5544, #9322, #805 ),
 ( #4598, #3667, #7349 ),
 ( #3786, #12276, #5667 ),
 ( #930, #7413, #7529 ),
 ( #8270, #11337, #6416 ),
 ( #2727, #2665, #8513 ),
 ( #7588, #9446, #11149 ),
 ( #4720, #11399, #9263 ),
 ( #9507, #11589, #5040 ),
 ( #1978, #3974, #8818 ),
 ( #10638, #10578, #6907 ),
 ( #3917, #4917, #8700 ),
 ( #2107, #3850, #1173 ),
 ( #11707, #6777, #3038 ),
 ( #3159, #6842, #7713 ),
 ( #7771, #5729, #988 ),
 ( #229, #7651, #5788 ),
 ( #1233, #4849, #11525 ),
 ( #1111, #8636, #10453 ),
 ( #4038, #11464, #4974 ),
 ( #4782, #2165, #164 ),
 ( #5910, #8573, #10698 ),
 ( #287, #9695, #9572 ),
 ( #8759, #4096, #7831 ),
 ( #11649, #7888, #36 ),
 ( #2043, #5968, #2978 ) ),
 .UNSPECIFIED., .F., .F., .F. ) 
 B_SPLINE_SURFACE_WITH_KNOTS ( ( 4, 2, 2, 2, 2, 2, 2, 2, 2, 2, 2, 2, 4 ),
 ( 3, 3 ),
 ( 0.006382978049045519471, 0.008387885753076820827, 0.009390339605092470204, 0.01039279345710812132, 0.01239770116113942180, 0.01340015501315507118, 0.01440260886517072229, 0.01540506271718637341, 0.01640751656920202278, 0.01841242427323332501, 0.01941487812524897438, 0.02041733197726462723, 0.02242223968129592598 ),
 ( 0.000000000000000000, 1.000000000000000000 ),
 .UNSPECIFIED. ) 
 GEOMETRIC_REPRESENTATION_ITEM ( )  RATIONAL_B_SPLINE_SURFACE ( (
 ( 1.000000000000000000, 0.8291561975888499525, 1.000000000000000000),
 ( 1.000000000000000000, 0.8291533992853002966, 1.000000000000000000),
 ( 1.000000000000000000, 0.8281244206747362391, 1.000000000000000000),
 ( 1.000000000000000000, 0.8251351734919084580, 1.000000000000000000),
 ( 1.000000000000000000, 0.8238971056969858209, 1.000000000000000000),
 ( 1.000000000000000000, 0.8209398665854176214, 1.000000000000000000),
 ( 1.000000000000000000, 0.8192278287709251483, 1.000000000000000000),
 ( 1.000000000000000000, 0.8135208904818415077, 1.000000000000000000),
 ( 1.000000000000000000, 0.8089311958809365377, 1.000000000000000000),
 ( 1.000000000000000000, 0.8010155071010215400, 1.000000000000000000),
 ( 1.000000000000000000, 0.7981992791123722064, 1.000000000000000000),
 ( 1.000000000000000000, 0.7923673440970026016, 1.000000000000000000),
 ( 1.000000000000000000, 0.7893380284540298941, 1.000000000000000000),
 ( 1.000000000000000000, 0.7830853791993543922, 1.000000000000000000),
 ( 1.000000000000000000, 0.7798619748040643840, 1.000000000000000000),
 ( 1.000000000000000000, 0.7732488416061723546, 1.000000000000000000),
 ( 1.000000000000000000, 0.7698413672832561394, 1.000000000000000000),
 ( 1.000000000000000000, 0.7595660318243934173, 1.000000000000000000),
 ( 1.000000000000000000, 0.7526475626047379741, 1.000000000000000000),
 ( 1.000000000000000000, 0.7423381171275357238, 1.000000000000000000),
 ( 1.000000000000000000, 0.7389127554685743782, 1.000000000000000000),
 ( 1.000000000000000000, 0.7321112719850653150, 1.000000000000000000),
 ( 1.000000000000000000, 0.7287565628962849873, 1.000000000000000000),
 ( 1.000000000000000000, 0.7189979416186721428, 1.000000000000000000),
 ( 1.000000000000000000, 0.7128432726192915903, 1.000000000000000000),
 ( 1.000000000000000000, 0.7071067811865474617, 1.000000000000000000) ) ) 
 REPRESENTATION_ITEM ( '' )  SURFACE ( )  );
#3219 = FILL_AREA_STYLE_COLOUR ( '', #11286 ) ;
#3220 = AXIS2_PLACEMENT_3D ( 'NONE', #536, #7211, #8260 ) ;
#3221 = CARTESIAN_POINT ( 'NONE',  ( -82.90657655639077461, 285.0000000000000568, 79.06642500897154946 ) ) ;
#3222 = DIRECTION ( 'NONE',  ( -0.000000000000000000, 0.8660254037844392627, 0.4999999999999990008 ) ) ;
#3223 = DIRECTION ( 'NONE',  ( 1.000000000000000000, -0.000000000000000000, 0.000000000000000000 ) ) ;
#3224 = CARTESIAN_POINT ( 'NONE',  ( 2.500000000000000000, 2.357898499370431722, -2.818925648462311528E-15 ) ) ;
#3225 = DIRECTION ( 'NONE',  ( 0.000000000000000000, -0.000000000000000000, 1.000000000000000000 ) ) ;
#3226 = EDGE_CURVE ( 'NONE', #80, #10035, #11498, .T. ) ;
#3227 = ADVANCED_FACE ( 'NONE', ( #10940 ), #2399, .T. ) ;
#3228 = CARTESIAN_POINT ( 'NONE',  ( -1.121994411437818862, 113.6249999986344079, 2.708734125000000326 ) ) ;
#3229 = VERTEX_POINT ( 'NONE', #5219 ) ;
#3230 = ADVANCED_FACE ( 'NONE', ( #2117 ), #6212, .F. ) ;
#3231 = VERTEX_POINT ( 'NONE', #3110 ) ;
#3232 = CARTESIAN_POINT ( 'NONE',  ( 29.05832229253450549, 87.09380371750550864, 8.606096436291641893 ) ) ;
#3233 = EDGE_LOOP ( 'NONE', ( #12284, #8659, #6992, #1185 ) ) ;
#3234 = CARTESIAN_POINT ( 'NONE',  ( 75.19960992036260450, 16.56778241586094680, -23.64972750892604125 ) ) ;
#3235 = EDGE_LOOP ( 'NONE', ( #11961, #3542, #2491, #1580 ) ) ;
#3236 = CIRCLE ( 'NONE', #6618, 5.000000000000007105 ) ;
#3237 = DIRECTION ( 'NONE',  ( -0.000000000000000000, -1.000000000000000000, -0.000000000000000000 ) ) ;
#3238 = CARTESIAN_POINT ( 'NONE',  ( -28.78580657183879765, 87.64875042622799128, -9.783922737503317535 ) ) ;
#3239 = ORIENTED_EDGE ( 'NONE', *, *, #1370, .F. ) ;
#3240 = CARTESIAN_POINT ( 'NONE',  ( 69.71747094087790231, 43.20762629113575315, -27.65023488237562788 ) ) ;
#3241 = ORIENTED_EDGE ( 'NONE', *, *, #1958, .T. ) ;
#3242 = DIRECTION ( 'NONE',  ( 0.000000000000000000, 0.000000000000000000, 1.000000000000000000 ) ) ;
#3243 = DIRECTION ( 'NONE',  ( 0.000000000000000000, 0.000000000000000000, 1.000000000000000000 ) ) ;
#3244 = ORIENTED_EDGE ( 'NONE', *, *, #8505, .F. ) ;
#3245 = CARTESIAN_POINT ( 'NONE',  ( 3.245314017740474622E-16, 170.0000000000000000, -2.649999999999987477 ) ) ;
#3246 = CARTESIAN_POINT ( 'NONE',  ( 71.93667174376723494, 10.34708426542594140, 21.21818801319905745 ) ) ;
#3247 = ORIENTED_EDGE ( 'NONE', *, *, #11041, .T. ) ;
#3248 = CARTESIAN_POINT ( 'NONE',  ( 0.000000000000000000, -5.000000000000000000, 70.00000000000001421 ) ) ;
#3249 = DIRECTION ( 'NONE',  ( 0.000000000000000000, 0.000000000000000000, -1.000000000000000000 ) ) ;
#3250 = CARTESIAN_POINT ( 'NONE',  ( 140.0000000000011369, 30.00000000000008882, 25.00000000000000000 ) ) ;
#3251 = CIRCLE ( 'NONE', #4048, 45.00000000000000000 ) ;
#3252 = ORIENTED_EDGE ( 'NONE', *, *, #7895, .F. ) ;
#3253 = DIRECTION ( 'NONE',  ( -1.000000000000000000, 0.000000000000000000, 0.000000000000000000 ) ) ;
#3254 = EDGE_CURVE ( 'NONE', #7160, #2064, #7135, .T. ) ;
#3255 = CARTESIAN_POINT ( 'NONE',  ( 75.38685631124154440, 16.31864566613397471, 23.38733102174731471 ) ) ;
#3256 = VERTEX_POINT ( 'NONE', #6270 ) ;
#3257 = CARTESIAN_POINT ( 'NONE',  ( 72.45695464226038496, 45.13428099848909625, -19.37542581275873843 ) ) ;
#3258 = CARTESIAN_POINT ( 'NONE',  ( -30.00100000000000122, 85.26794919243110371, 9.660254037844429931 ) ) ;
#3259 = CIRCLE ( 'NONE', #10222, 15.00000000000000000 ) ;
#3260 = EDGE_LOOP ( 'NONE', ( #3091, #2073, #3433, #7906, #2871 ) ) ;
#3261 = DIRECTION ( 'NONE',  ( 0.000000000000000000, -1.000000000000000000, 0.000000000000000000 ) ) ;
#3262 = CARTESIAN_POINT ( 'NONE',  ( 69.73318542092245309, 43.28701116280399219, 27.60965287711969651 ) ) ;
#3263 = ORIENTED_EDGE ( 'NONE', *, *, #6982, .T. ) ;
#3264 = DIRECTION ( 'NONE',  ( 1.000000000000000000, -1.387778780781445676E-14, 0.000000000000000000 ) ) ;
#3265 = CARTESIAN_POINT ( 'NONE',  ( -89.80805993797480369, 275.0000000000000000, 81.82974571984181011 ) ) ;
#3266 = DIRECTION ( 'NONE',  ( 0.000000000000000000, 1.000000000000000000, 0.000000000000000000 ) ) ;
#3267 = CARTESIAN_POINT ( 'NONE',  ( -1.915364268218909150, 113.6874999986344079, 1.915364268218909594 ) ) ;
#3268 = EDGE_CURVE ( 'NONE', #893, #4148, #8996, .T. ) ;
#3269 = EDGE_CURVE ( 'NONE', #10685, #7290, #8719, .T. ) ;
#3270 = VERTEX_POINT ( 'NONE', #9703 ) ;
#3271 = AXIS2_PLACEMENT_3D ( 'NONE', #5451, #6134, #7321 ) ;
#3272 = VERTEX_POINT ( 'NONE', #9060 ) ;
#3273 = VECTOR ( 'NONE', #10824, 1000.000000000000000 ) ;
#3274 = ORIENTED_EDGE ( 'NONE', *, *, #3662, .T. ) ;
#3275 = EDGE_CURVE ( 'NONE', #2274, #11587, #7840, .T. ) ;
#3276 = CARTESIAN_POINT ( 'NONE',  ( 135.0000000000011084, 67.07106781186550393, 20.00000000000000000 ) ) ;
#3277 = DIRECTION ( 'NONE',  ( 1.000000000000000000, 0.000000000000000000, 0.000000000000000000 ) ) ;
#3278 = AXIS2_PLACEMENT_3D ( 'NONE', #3052, #6856, #7099 ) ;
#3279 = CARTESIAN_POINT ( 'NONE',  ( 26.76795759904968364, 61.76795759904965877, -64.77864552555394084 ) ) ;
#3280 = AXIS2_PLACEMENT_3D ( 'NONE', #2008, #5815, #2245 ) ;
#3281 = LINE ( 'NONE', #1413, #302 ) ;
#3282 = CARTESIAN_POINT ( 'NONE',  ( 0.000000000000000000, 115.0000000000000000, 0.000000000000000000 ) ) ;
#3283 = CONTEXT_DEPENDENT_SHAPE_REPRESENTATION ( #11710, #9449 ) ;
#3284 = EDGE_CURVE ( 'NONE', #11288, #11474, #566, .T. ) ;
#3285 = EDGE_CURVE ( 'NONE', #7839, #8096, #7998, .T. ) ;
#3286 = DIRECTION ( 'NONE',  ( -1.000000000000000000, 0.000000000000000000, -0.000000000000000000 ) ) ;
#3287 = CARTESIAN_POINT ( 'NONE',  ( -1.915364268218909816, 112.9374999986344079, -1.915364268218909150 ) ) ;
#3288 = ORIENTED_EDGE ( 'NONE', *, *, #2648, .T. ) ;
#3289 = DIRECTION ( 'NONE',  ( -0.4999999999999977796, 0.8660254037844399289, 0.000000000000000000 ) ) ;
#3290 = VECTOR ( 'NONE', #11008, 1000.000000000000000 ) ;
#3291 = VECTOR ( 'NONE', #5624, 1000.000000000000000 ) ;
#3292 = ORIENTED_EDGE ( 'NONE', *, *, #7210, .T. ) ;
#3293 = EDGE_CURVE ( 'NONE', #5680, #4162, #594, .T. ) ;
#3294 = CARTESIAN_POINT ( 'NONE',  ( 29.00531465893917371, 86.42397445337759621, 8.992822542244239159 ) ) ;
#3295 = EDGE_LOOP ( 'NONE', ( #4189, #2130, #5304, #1286, #1935, #6985, #2168 ) ) ;
#3296 = DIRECTION ( 'NONE',  ( 0.000000000000000000, 0.000000000000000000, 1.000000000000000000 ) ) ;
#3297 = CARTESIAN_POINT ( 'NONE',  ( -5.970153145843347347E-16, 113.6249999972688158, -3.250000000000000444 ) ) ;
#3298 = ORIENTED_EDGE ( 'NONE', *, *, #2280, .F. ) ;
#3299 = AXIS2_PLACEMENT_3D ( 'NONE', #9721, #257, #131 ) ;
#3300 = DIRECTION ( 'NONE',  ( 0.4999999999999985012, 0.8660254037844394848, 0.000000000000000000 ) ) ;
#3301 = CARTESIAN_POINT ( 'NONE',  ( 145.0000000000011369, 225.0000000000000853, 20.00000000000000000 ) ) ;
#3302 = ORIENTED_EDGE ( 'NONE', *, *, #927, .T. ) ;
#3303 = CARTESIAN_POINT ( 'NONE',  ( -2.298097038856279806, 113.6250000000000000, -2.298097038856279362 ) ) ;
#3304 = AXIS2_PLACEMENT_3D ( 'NONE', #3171, #4053, #7844 ) ;
#3305 = AXIS2_PLACEMENT_3D ( 'NONE', #9278, #11039, #5620 ) ;
#3306 = AXIS2_PLACEMENT_3D ( 'NONE', #6146, #4031, #11768 ) ;
#3307 = ORIENTED_EDGE ( 'NONE', *, *, #6439, .F. ) ;
#3308 = EDGE_CURVE ( 'NONE', #2099, #3401, #12317, .T. ) ;
#3309 = DIRECTION ( 'NONE',  ( 0.000000000000000000, 1.000000000000000000, 0.000000000000000000 ) ) ;
#3310 = CARTESIAN_POINT ( 'NONE',  ( 0.000000000000000000, 10.00000000000017586, 0.000000000000000000 ) ) ;
#3311 = ORIENTED_EDGE ( 'NONE', *, *, #3420, .T. ) ;
#3312 = VECTOR ( 'NONE', #1465, 1000.000000000000000 ) ;
#3313 = CARTESIAN_POINT ( 'NONE',  ( 0.000000000000000000, 285.0000000000000568, 0.000000000000000000 ) ) ;
#3314 = FACE_OUTER_BOUND ( 'NONE', #2939, .T. ) ;
#3315 = ORIENTED_EDGE ( 'NONE', *, *, #11692, .T. ) ;
#3316 = SHAPE_REPRESENTATION ( 'Clear Processing Bowl', ( #1612 ), #1360 ) ;
#3317 = CARTESIAN_POINT ( 'NONE',  ( 2.500000000000000000, 2.357898499370431722, -2.818925648462311528E-15 ) ) ;
#3318 = DIRECTION ( 'NONE',  ( -0.000000000000000000, -1.000000000000000000, -0.000000000000000000 ) ) ;
#3319 = DIRECTION ( 'NONE',  ( 0.000000000000000000, 0.8660254037844380415, -0.5000000000000012212 ) ) ;
#3320 = ORIENTED_EDGE ( 'NONE', *, *, #8449, .F. ) ;
#3321 = LINE ( 'NONE', #7060, #2586 ) ;
#3322 = CARTESIAN_POINT ( 'NONE',  ( 76.19556706709904859, 15.49470566993306520, 22.19251267860115462 ) ) ;
#3323 = VECTOR ( 'NONE', #8306, 1000.000000000000000 ) ;
#3324 = ORIENTED_EDGE ( 'NONE', *, *, #609, .T. ) ;
#3325 = CARTESIAN_POINT ( 'NONE',  ( 72.53968727264539496, 45.08133313514087348, -19.05499925486959256 ) ) ;
#3326 = DIRECTION ( 'NONE',  ( -0.000000000000000000, -1.000000000000000000, -0.000000000000000000 ) ) ;
#3327 = ORIENTED_EDGE ( 'NONE', *, *, #11690, .T. ) ;
#3328 = DIRECTION ( 'NONE',  ( 0.000000000000000000, -0.000000000000000000, 1.000000000000000000 ) ) ;
#3329 = CARTESIAN_POINT ( 'NONE',  ( 69.91894869711104832, 44.51764890176950473, 27.13685080543958250 ) ) ;
#3330 = ORIENTED_EDGE ( 'NONE', *, *, #6412, .F. ) ;
#3331 = EDGE_CURVE ( 'NONE', #7839, #934, #2710, .T. ) ;
#3332 = DIRECTION ( 'NONE',  ( 0.000000000000000000, 1.000000000000000000, 0.000000000000000000 ) ) ;
#3333 = CARTESIAN_POINT ( 'NONE',  ( 6.000000000000000000, 62.00000000000000000, 69.74238309665078361 ) ) ;
#3334 = EDGE_CURVE ( 'NONE', #4135, #10304, #3586, .T. ) ;
#3335 = DIRECTION ( 'NONE',  ( 0.000000000000000000, 1.000000000000000000, 0.000000000000000000 ) ) ;
#3336 = CARTESIAN_POINT ( 'NONE',  ( -4.975863863883684959E-16, 113.0624999986344079, -2.708734125000000326 ) ) ;
#3337 = ORIENTED_EDGE ( 'NONE', *, *, #10324, .T. ) ;
#3338 = ORIENTED_EDGE ( 'NONE', *, *, #7548, .F. ) ;
#3339 =( LENGTH_UNIT ( ) NAMED_UNIT ( * ) SI_UNIT ( .MILLI., .METRE. ) );
#3340 = VERTEX_POINT ( 'NONE', #10308 ) ;
#3341 = DIRECTION ( 'NONE',  ( -6.938893903907222067E-15, -1.000000000000000000, 0.000000000000000000 ) ) ;
#3342 = DIRECTION ( 'NONE',  ( 0.000000000000000000, 0.000000000000000000, 1.000000000000000000 ) ) ;
#3343 = ADVANCED_FACE ( 'NONE', ( #4524 ), #11327, .F. ) ;
#3344 = EDGE_CURVE ( 'NONE', #4721, #3517, #5947, .T. ) ;
#3345 = LINE ( 'NONE', #2340, #4651 ) ;
#3346 = CARTESIAN_POINT ( 'NONE',  ( 20.00000000000000000, 54.99999999999999289, -67.08203932499371547 ) ) ;
#3347 = CARTESIAN_POINT ( 'NONE',  ( -12.57411137850303540, 36.28349364905398033, 80.00000000000000000 ) ) ;
#3348 = DIRECTION ( 'NONE',  ( 2.213536252433181072E-16, 0.000000000000000000, 1.000000000000000000 ) ) ;
#3349 = AXIS2_PLACEMENT_3D ( 'NONE', #10588, #2927, #10524 ) ;
#3350 = LINE ( 'NONE', #12143, #10779 ) ;
#3351 = CARTESIAN_POINT ( 'NONE',  ( 72.45461974811382788, 10.00000000000009592, -19.38446435976419835 ) ) ;
#3352 = EDGE_CURVE ( 'NONE', #5980, #1372, #11131, .T. ) ;
#3353 = CARTESIAN_POINT ( 'NONE',  ( -2.708734125000000326, 113.7499999986343937, 1.121994411437818862 ) ) ;
#3354 = CARTESIAN_POINT ( 'NONE',  ( 10.19254911989241386, 23.71650635094626836, 79.50000000000000000 ) ) ;
#3355 = CARTESIAN_POINT ( 'NONE',  ( 109.9268209223821628, 275.0000000000000000, 32.26598893414752212 ) ) ;
#3356 = AXIS2_PLACEMENT_3D ( 'NONE', #6331, #1473, #5278 ) ;
#3357 = EDGE_CURVE ( 'NONE', #5022, #9737, #12322, .T. ) ;
#3358 = ADVANCED_FACE ( 'NONE', ( #12200, #6458 ), #5650, .T. ) ;
#3359 =( GEOMETRIC_REPRESENTATION_CONTEXT ( 3 ) GLOBAL_UNCERTAINTY_ASSIGNED_CONTEXT ( ( #4390 ) ) GLOBAL_UNIT_ASSIGNED_CONTEXT ( ( #1532, #6144, #8000 ) ) REPRESENTATION_CONTEXT ( 'NONE', 'WORKASPACE' ) );
#3360 = ORIENTED_EDGE ( 'NONE', *, *, #7641, .F. ) ;
#3361 = LINE ( 'NONE', #7156, #7825 ) ;
#3362 = ORIENTED_EDGE ( 'NONE', *, *, #11281, .F. ) ;
#3363 = FACE_OUTER_BOUND ( 'NONE', #10278, .T. ) ;
#3364 = CARTESIAN_POINT ( 'NONE',  ( -89.80805993797480369, 275.0000000000000000, 71.82974571984181011 ) ) ;
#3365 = ORIENTED_EDGE ( 'NONE', *, *, #7691, .F. ) ;
#3366 = CARTESIAN_POINT ( 'NONE',  ( 27.32050286291078933, 86.95679894682506017, 12.39317045950328300 ) ) ;
#3367 = CARTESIAN_POINT ( 'NONE',  ( -28.61611180472258553, 87.72948999988449259, -9.923767781257849308 ) ) ;
#3368 = VERTEX_POINT ( 'NONE', #7573 ) ;
#3369 = CARTESIAN_POINT ( 'NONE',  ( 69.64721689463591758, 42.58935033937477499, -27.82591776719579357 ) ) ;
#3370 = VERTEX_POINT ( 'NONE', #10246 ) ;
#3371 = DIRECTION ( 'NONE',  ( -0.000000000000000000, -1.000000000000000000, -0.000000000000000000 ) ) ;
#3372 = DIRECTION ( 'NONE',  ( -0.000000000000000000, 1.000000000000000000, -0.000000000000000000 ) ) ;
#3373 = CIRCLE ( 'NONE', #2396, 28.00000000000000355 ) ;
#3374 = ORIENTED_EDGE ( 'NONE', *, *, #1598, .T. ) ;
#3375 = CARTESIAN_POINT ( 'NONE',  ( 10.19254911989241386, 23.71650635094626836, 79.50000000000000000 ) ) ;
#3376 = DIRECTION ( 'NONE',  ( -3.469446951953613203E-16, 0.000000000000000000, -1.000000000000000000 ) ) ;
#3377 = ORIENTED_EDGE ( 'NONE', *, *, #7141, .F. ) ;
#3378 = DIRECTION ( 'NONE',  ( 0.000000000000000000, 0.000000000000000000, 1.000000000000000000 ) ) ;
#3379 = DIRECTION ( 'NONE',  ( -0.7071067811865433539, 0.7071067811865517916, 0.000000000000000000 ) ) ;
#3380 = LINE ( 'NONE', #7245, #1820 ) ;
#3381 = EDGE_LOOP ( 'NONE', ( #12170, #10802, #290, #3617 ) ) ;
#3382 = CARTESIAN_POINT ( 'NONE',  ( 1.915364268218909150, 110.6874999986344079, 1.915364268218909150 ) ) ;
#3383 = ADVANCED_FACE ( 'NONE', ( #11383 ), #1722, .T. ) ;
#3384 = EDGE_CURVE ( 'NONE', #5113, #712, #2350, .T. ) ;
#3385 = CARTESIAN_POINT ( 'NONE',  ( 70.75630133281157441, 12.41939062735542976, 24.87185742758358487 ) ) ;
#3386 = VECTOR ( 'NONE', #3607, 1000.000000000000000 ) ;
#3387 = EDGE_CURVE ( 'NONE', #7990, #2747, #6393, .T. ) ;
#3388 = VERTEX_POINT ( 'NONE', #1901 ) ;
#3389 = CARTESIAN_POINT ( 'NONE',  ( -7.907287480251421030, 41.13333024919781167, 79.50000000000000000 ) ) ;
#3390 = FACE_OUTER_BOUND ( 'NONE', #4413, .T. ) ;
#3391 = ORIENTED_EDGE ( 'NONE', *, *, #9205, .F. ) ;
#3392 = LINE ( 'NONE', #9167, #5868 ) ;
#3393 = CARTESIAN_POINT ( 'NONE',  ( 75.47443053502085775, 43.79154879885060581, 23.26350036030316559 ) ) ;
#3394 = ORIENTED_EDGE ( 'NONE', *, *, #1836, .T. ) ;
#3395 = CARTESIAN_POINT ( 'NONE',  ( 0.000000000000000000, 335.0000000000000000, 0.000000000000000000 ) ) ;
#3396 = AXIS2_PLACEMENT_3D ( 'NONE', #6373, #4310, #4434 ) ;
#3397 = DIRECTION ( 'NONE',  ( 1.000000000000000000, -0.000000000000000000, 1.224646799147353207E-16 ) ) ;
#3398 = PLANE ( 'NONE',  #11169 ) ;
#3399 = VERTEX_POINT ( 'NONE', #2834 ) ;
#3400 = ORIENTED_EDGE ( 'NONE', *, *, #9873, .T. ) ;
#3401 = VERTEX_POINT ( 'NONE', #8496 ) ;
#3402 = AXIS2_PLACEMENT_3D ( 'NONE', #1952, #5579, #5703 ) ;
#3403 = AXIS2_PLACEMENT_3D ( 'NONE', #1357, #7095, #7216 ) ;
#3404 = VECTOR ( 'NONE', #4142, 1000.000000000000000 ) ;
#3405 = UNCERTAINTY_MEASURE_WITH_UNIT (LENGTH_MEASURE( 1.000000000000000082E-05 ), #8494, 'distance_accuracy_value', 'NONE');
#3406 = CARTESIAN_POINT ( 'NONE',  ( -6.407287480251391720, 21.46474596215567487, 79.50000000000000000 ) ) ;
#3407 = DIRECTION ( 'NONE',  ( 0.000000000000000000, 0.000000000000000000, 1.000000000000000000 ) ) ;
#3408 = DIRECTION ( 'NONE',  ( 0.000000000000000000, 1.224646799147353207E-16, 1.000000000000000000 ) ) ;
#3409 = DIRECTION ( 'NONE',  ( 0.000000000000000000, -1.000000000000000000, -0.000000000000000000 ) ) ;
#3410 = LINE ( 'NONE', #7208, #3290 ) ;
#3411 = AXIS2_PLACEMENT_3D ( 'NONE', #1384, #12050, #1573 ) ;
#3412 = CARTESIAN_POINT ( 'NONE',  ( 31.68100721119781937, 75.82462385531685811, -6.696065238440062295 ) ) ;
#3413 = VECTOR ( 'NONE', #12115, 1000.000000000000227 ) ;
#3414 = CARTESIAN_POINT ( 'NONE',  ( 5.525725221640833240, 18.86666975080242992, 79.50000000000000000 ) ) ;
#3415 = CARTESIAN_POINT ( 'NONE',  ( 70.19857488179017935, 14.21697453379132803, -26.40439979598029652 ) ) ;
#3416 = CARTESIAN_POINT ( 'NONE',  ( 2.708734125000000326, 112.3124999986344079, 0.000000000000000000 ) ) ;
#3417 = CARTESIAN_POINT ( 'NONE',  ( -14.18837706086142703, 30.25000000000008882, 80.00000000000000000 ) ) ;
#3418 = DIRECTION ( 'NONE',  ( 0.8660254037844434816, 0.4999999999999913958, 0.000000000000000000 ) ) ;
#3419 = AXIS2_PLACEMENT_3D ( 'NONE', #5370, #10033, #9088 ) ;
#3420 = EDGE_CURVE ( 'NONE', #6532, #2361, #10111, .T. ) ;
#3421 = AXIS2_PLACEMENT_3D ( 'NONE', #9941, #7277, #2536 ) ;
#3422 = VERTEX_POINT ( 'NONE', #6639 ) ;
#3423 = CARTESIAN_POINT ( 'NONE',  ( 28.82113438502227609, 85.77482169911409926, 9.367611059682538155 ) ) ;
#3424 = ORIENTED_EDGE ( 'NONE', *, *, #5151, .T. ) ;
#3425 = DIRECTION ( 'NONE',  ( 1.224646799147352961E-16, 0.000000000000000000, -1.000000000000000000 ) ) ;
#3426 = DIRECTION ( 'NONE',  ( 0.9595199576812829534, 0.000000000000000000, -0.2816406412634883671 ) ) ;
#3427 = VERTEX_POINT ( 'NONE', #7455 ) ;
#3428 = AXIS2_PLACEMENT_3D ( 'NONE', #8939, #7829, #5039 ) ;
#3429 = FACE_OUTER_BOUND ( 'NONE', #11155, .T. ) ;
#3430 = AXIS2_PLACEMENT_3D ( 'NONE', #12017, #4462, #11954 ) ;
#3431 = DIRECTION ( 'NONE',  ( 1.000000000000000000, -0.000000000000000000, 0.000000000000000000 ) ) ;
#3432 = EDGE_CURVE ( 'NONE', #1442, #6428, #6343, .T. ) ;
#3433 = ORIENTED_EDGE ( 'NONE', *, *, #10409, .T. ) ;
#3434 = ADVANCED_FACE ( 'NONE', ( #11265 ), #5712, .F. ) ;
#3435 = CARTESIAN_POINT ( 'NONE',  ( 71.75867793008814033, 49.45719000729793891, -21.81257403104604720 ) ) ;
#3436 = VERTEX_POINT ( 'NONE', #5463 ) ;
#3437 = VECTOR ( 'NONE', #4645, 1000.000000000000000 ) ;
#3438 = DIRECTION ( 'NONE',  ( 0.000000000000000000, 0.000000000000000000, 1.000000000000000000 ) ) ;
#3439 = FACE_OUTER_BOUND ( 'NONE', #5328, .T. ) ;
#3440 = VERTEX_POINT ( 'NONE', #9244 ) ;
#3441 = EDGE_LOOP ( 'NONE', ( #989, #4417, #1324, #6599, #562 ) ) ;
#3442 = DIRECTION ( 'NONE',  ( 0.000000000000000000, 1.000000000000000000, 0.000000000000000000 ) ) ;
#3443 = CARTESIAN_POINT ( 'NONE',  ( 71.40042903152234999, 11.04265768716983054, 22.96380533506443555 ) ) ;
#3444 = ORIENTED_EDGE ( 'NONE', *, *, #7986, .T. ) ;
#3445 = DIRECTION ( 'NONE',  ( 0.000000000000000000, 0.000000000000000000, 1.000000000000000000 ) ) ;
#3446 = DIRECTION ( 'NONE',  ( 0.000000000000000000, 0.000000000000000000, 1.000000000000000000 ) ) ;
#3447 = DIRECTION ( 'NONE',  ( -0.000000000000000000, -1.000000000000000000, -0.000000000000000000 ) ) ;
#3448 = VERTEX_POINT ( 'NONE', #2088 ) ;
#3449 = CARTESIAN_POINT ( 'NONE',  ( 74.70719529697694838, 17.45645769019468574, 24.30790125104220678 ) ) ;
#3450 = VERTEX_POINT ( 'NONE', #1277 ) ;
#3451 = DIRECTION ( 'NONE',  ( 0.000000000000000000, 1.000000000000000000, 0.000000000000000000 ) ) ;
#3452 = CARTESIAN_POINT ( 'NONE',  ( -1.440781129305261477, 20.00000000000009592, 79.50000000000000000 ) ) ;
#3453 = ORIENTED_EDGE ( 'NONE', *, *, #3200, .T. ) ;
#3454 = EDGE_CURVE ( 'NONE', #867, #434, #8685, .T. ) ;
#3455 = CARTESIAN_POINT ( 'NONE',  ( 74.18968745904427919, 40.67159320117693966, 24.96588476870680751 ) ) ;
#3456 = CIRCLE ( 'NONE', #9811, 45.00000000000000000 ) ;
#3457 = EDGE_LOOP ( 'NONE', ( #6158, #8853 ) ) ;
#3458 = CARTESIAN_POINT ( 'NONE',  ( 8.572527594031472993E-15, 65.00000000000000000, -70.00000000000000000 ) ) ;
#3459 = DIRECTION ( 'NONE',  ( 0.000000000000000000, 1.000000000000000000, 0.000000000000000000 ) ) ;
#3460 = CARTESIAN_POINT ( 'NONE',  ( 1.121994411437819528, 113.1249999986344079, -2.708734124999999882 ) ) ;
#3461 = EDGE_LOOP ( 'NONE', ( #10813, #8441, #1881 ) ) ;
#3462 =( NAMED_UNIT ( * ) SI_UNIT ( $, .STERADIAN. ) SOLID_ANGLE_UNIT ( ) );
#3463 = ORIENTED_EDGE ( 'NONE', *, *, #11291, .F. ) ;
#3464 = AXIS2_PLACEMENT_3D ( 'NONE', #8997, #7085, #3277 ) ;
#3465 = VECTOR ( 'NONE', #1961, 1000.000000000000000 ) ;
#3466 = FACE_OUTER_BOUND ( 'NONE', #1897, .T. ) ;
#3467 = CARTESIAN_POINT ( 'NONE',  ( 167.9289321881357182, 35.85786437626914847, -25.00000000000001066 ) ) ;
#3468 = CYLINDRICAL_SURFACE ( 'NONE', #1248, 100.0000000000000284 ) ;
#3469 = FACE_OUTER_BOUND ( 'NONE', #9577, .T. ) ;
#3470 = CARTESIAN_POINT ( 'NONE',  ( -8.000000000000000000, 115.0000000000000000, -5.999999999999998224 ) ) ;
#3471 = CARTESIAN_POINT ( 'NONE',  ( -12.12726286035689327, 40.31710753316119877, 74.01694684401550717 ) ) ;
#3472 = CARTESIAN_POINT ( 'NONE',  ( 9.183067057334849181, 19.15551980836006152, 74.43651270773197837 ) ) ;
#3473 = CARTESIAN_POINT ( 'NONE',  ( 69.65097664248530407, 17.43447699930461425, -27.81636932325740474 ) ) ;
#3474 = VECTOR ( 'NONE', #8261, 1000.000000000000114 ) ;
#3475 = CARTESIAN_POINT ( 'NONE',  ( 3.250000000000000444, 113.0625000000000000, 1.346194077712559389 ) ) ;
#3476 = CARTESIAN_POINT ( 'NONE',  ( 0.000000000000000000, 340.0000000000000000, 0.000000000000000000 ) ) ;
#3477 = DIRECTION ( 'NONE',  ( 0.000000000000000000, 0.000000000000000000, 1.000000000000000000 ) ) ;
#3478 = AXIS2_PLACEMENT_3D ( 'NONE', #10231, #5695, #8419 ) ;
#3479 = EDGE_LOOP ( 'NONE', ( #8081, #6491 ) ) ;
#3480 = DIRECTION ( 'NONE',  ( 0.000000000000000000, 0.000000000000000000, 1.000000000000000000 ) ) ;
#3481 = EDGE_LOOP ( 'NONE', ( #9272, #8524, #11564, #10594, #3453 ) ) ;
#3482 = CARTESIAN_POINT ( 'NONE',  ( -7.835118696620823719, 18.82500308414615731, 80.00000048127353125 ) ) ;
#3483 = CARTESIAN_POINT ( 'NONE',  ( 75.52936542331363512, 16.13405212679771239, -23.18670291617644708 ) ) ;
#3484 = ORIENTED_EDGE ( 'NONE', *, *, #1288, .F. ) ;
#3485 = ADVANCED_FACE ( 'NONE', ( #2147, #7695 ), #8622, .T. ) ;
#3486 = DIRECTION ( 'NONE',  ( 0.8660254037844394848, 0.4999999999999985567, 0.000000000000000000 ) ) ;
#3487 = EDGE_CURVE ( 'NONE', #9722, #5183, #10575, .T. ) ;
#3488 = CARTESIAN_POINT ( 'NONE',  ( 0.000000000000000000, 65.00000000000000000, -72.00000000000002842 ) ) ;
#3489 = ORIENTED_EDGE ( 'NONE', *, *, #8664, .T. ) ;
#3490 = PLANE ( 'NONE',  #6172 ) ;
#3491 = AXIS2_PLACEMENT_3D ( 'NONE', #7846, #2060, #1129 ) ;
#3492 = EDGE_LOOP ( 'NONE', ( #851, #7800, #9621, #7866, #3063 ) ) ;
#3493 = DIRECTION ( 'NONE',  ( -1.000000000000000000, 0.000000000000000000, 0.000000000000000000 ) ) ;
#3494 = DIRECTION ( 'NONE',  ( 0.000000000000000000, -0.000000000000000000, 1.000000000000000000 ) ) ;
#3495 = ORIENTED_EDGE ( 'NONE', *, *, #1623, .T. ) ;
#3496 = VECTOR ( 'NONE', #8006, 1000.000000000000000 ) ;
#3497 = DIRECTION ( 'NONE',  ( 0.000000000000000000, 0.000000000000000000, 1.000000000000000000 ) ) ;
#3498 = FACE_OUTER_BOUND ( 'NONE', #4380, .T. ) ;
#3499 = ORIENTED_EDGE ( 'NONE', *, *, #4666, .T. ) ;
#3500 = ADVANCED_FACE ( 'NONE', ( #8802 ), #5833, .F. ) ;
#3501 = CARTESIAN_POINT ( 'NONE',  ( 0.000000000000000000, 0.000000000000000000, 0.000000000000000000 ) ) ;
#3502 = AXIS2_PLACEMENT_3D ( 'NONE', #845, #4638, #1893 ) ;
#3503 = DIRECTION ( 'NONE',  ( -0.000000000000000000, -1.000000000000000000, -0.000000000000000000 ) ) ;
#3504 = AXIS2_PLACEMENT_3D ( 'NONE', #4659, #10201, #677 ) ;
#3505 = CARTESIAN_POINT ( 'NONE',  ( 21.00000000000000000, 2.055000000000000160, 0.000000000000000000 ) ) ;
#3506 = DIRECTION ( 'NONE',  ( 3.469446951953611033E-15, 1.000000000000000000, 0.000000000000000000 ) ) ;
#3507 = EDGE_LOOP ( 'NONE', ( #7921, #2157 ) ) ;
#3508 = CARTESIAN_POINT ( 'NONE',  ( 7.344472908538985045, 35.21650635094629678, 79.50000000000000000 ) ) ;
#3509 = CARTESIAN_POINT ( 'NONE',  ( 74.16198487095664404, 20.00000000000009237, 25.00000000000000000 ) ) ;
#3510 = AXIS2_PLACEMENT_3D ( 'NONE', #1261, #10034, #4242 ) ;
#3511 = B_SPLINE_CURVE_WITH_KNOTS ( 'NONE', 3,
 ( #8357, #8300, #7440, #10294, #4627, #2753, #12243, #3690, #11307, #6561, #11552, #2133, #6056, #1014, #10786, #7910, #4815, #4880, #8603, #7677, #3879, #64, #1198, #1140, #9783, #5876, #5001, #7803 ),
 .UNSPECIFIED., .F., .F.,
 ( 4, 2, 2, 2, 2, 2, 2, 2, 2, 2, 2, 2, 2, 4 ),
 ( 0.06933356886758795801, 0.07087674937109647577, 0.07241992987460497966, 0.07396311037811349742, 0.07550629088162201519, 0.07859265188863905072, 0.08013583239214755460, 0.08167901289565607237, 0.08476537390267309402, 0.08630855440618159791, 0.08785173490969010179, 0.08939491541319860568, 0.09093809591670712345, 0.09402445692372414510 ),
 .UNSPECIFIED. ) ;
#3512 = ORIENTED_EDGE ( 'NONE', *, *, #596, .T. ) ;
#3513 = ADVANCED_FACE ( 'NONE', ( #271 ), #82, .T. ) ;
#3514 = DIRECTION ( 'NONE',  ( 0.000000000000000000, 0.000000000000000000, 1.000000000000000000 ) ) ;
#3515 = EDGE_CURVE ( 'NONE', #9969, #9385, #8064, .T. ) ;
#3516 = DIRECTION ( 'NONE',  ( 0.8660254037844434816, 0.4999999999999913958, 0.000000000000000000 ) ) ;
#3517 = VERTEX_POINT ( 'NONE', #6889 ) ;
#3518 = CARTESIAN_POINT ( 'NONE',  ( 1.346194077712564940, 110.8124999999999858, -3.249999999999993783 ) ) ;
#3519 = DIRECTION ( 'NONE',  ( -0.000000000000000000, 1.000000000000000000, -0.000000000000000000 ) ) ;
#3520 = ORIENTED_EDGE ( 'NONE', *, *, #2888, .T. ) ;
#3521 = CARTESIAN_POINT ( 'NONE',  ( -30.43816488677641630, 83.71535165408627677, -2.971076217724753832 ) ) ;
#3522 = CARTESIAN_POINT ( 'NONE',  ( 1.530808498934191127E-15, 115.0000000000000000, -9.999999999999998224 ) ) ;
#3523 = CARTESIAN_POINT ( 'NONE',  ( 2.708734125000000326, 113.3124999986344079, 0.000000000000000000 ) ) ;
#3524 = CARTESIAN_POINT ( 'NONE',  ( -1.121994411437820194, 113.2499999986344079, -2.708734124999999437 ) ) ;
#3525 = VECTOR ( 'NONE', #1204, 1000.000000000000114 ) ;
#3526 = ORIENTED_EDGE ( 'NONE', *, *, #248, .F. ) ;
#3527 = VERTEX_POINT ( 'NONE', #3959 ) ;
#3528 = AXIS2_PLACEMENT_3D ( 'NONE', #634, #5563, #9217 ) ;
#3529 = FACE_OUTER_BOUND ( 'NONE', #10150, .T. ) ;
#3530 = CARTESIAN_POINT ( 'NONE',  ( -30.50145854323920602, 85.38003226577613702, -9.854387615546507107 ) ) ;
#3531 = LINE ( 'NONE', #790, #3437 ) ;
#3532 = DIRECTION ( 'NONE',  ( 0.000000000000000000, -0.8660254037844402619, 0.4999999999999975575 ) ) ;
#3533 = FACE_OUTER_BOUND ( 'NONE', #6571, .T. ) ;
#3534 = CARTESIAN_POINT ( 'NONE',  ( -4.117654238873405426, 44.72076144782612772, 74.88857929402055902 ) ) ;
#3535 = CARTESIAN_POINT ( 'NONE',  ( -25.00000000000000000, 347.0000000000000568, -31.99999999999999289 ) ) ;
#3536 = CARTESIAN_POINT ( 'NONE',  ( 70.48329812536721306, 13.20517121183804043, -25.63505613512332815 ) ) ;
#3537 = EDGE_LOOP ( 'NONE', ( #5793, #9643, #8350, #7032, #6262 ) ) ;
#3538 = CARTESIAN_POINT ( 'NONE',  ( -3.250000000000000444, 113.4375000000000000, 1.346194077712559389 ) ) ;
#3539 = DIRECTION ( 'NONE',  ( -0.8660254037844403729, -0.4999999999999970024, 0.000000000000000000 ) ) ;
#3540 = EDGE_CURVE ( 'NONE', #4918, #9990, #9256, .T. ) ;
#3541 = EDGE_CURVE ( 'NONE', #366, #12281, #3104, .T. ) ;
#3542 = ORIENTED_EDGE ( 'NONE', *, *, #926, .T. ) ;
#3543 = DIRECTION ( 'NONE',  ( 0.000000000000000000, 0.000000000000000000, -1.000000000000000000 ) ) ;
#3544 = DIRECTION ( 'NONE',  ( 0.000000000000000000, 1.000000000000000000, 0.000000000000000000 ) ) ;
#3545 = CARTESIAN_POINT ( 'NONE',  ( -12.53244471184681075, 23.64433756731560266, 80.00000048127353125 ) ) ;
#3546 = ORIENTED_EDGE ( 'NONE', *, *, #5485, .F. ) ;
#3547 = CYLINDRICAL_SURFACE ( 'NONE', #1484, 4.999999999999997335 ) ;
#3548 = FACE_OUTER_BOUND ( 'NONE', #3872, .T. ) ;
#3549 = ORIENTED_EDGE ( 'NONE', *, *, #7403, .F. ) ;
#3550 = LINE ( 'NONE', #9270, #11560 ) ;
#3551 = AXIS2_PLACEMENT_3D ( 'NONE', #11475, #3861, #2053 ) ;
#3552 = VERTEX_POINT ( 'NONE', #10745 ) ;
#3553 = CARTESIAN_POINT ( 'NONE',  ( 34.84179752789421514, 75.25738092153642356, -7.654152443798540872 ) ) ;
#3555 = ORIENTED_EDGE ( 'NONE', *, *, #3004, .T. ) ;
#3554 = CYLINDRICAL_SURFACE ( 'NONE', #5641, 28.00000000000000355 ) ;
#3556 = ORIENTED_EDGE ( 'NONE', *, *, #1936, .T. ) ;
#3557 = CARTESIAN_POINT ( 'NONE',  ( 1.347111479062088996E-14, 335.0000000000000000, 110.0000000000000284 ) ) ;
#3558 = CARTESIAN_POINT ( 'NONE',  ( 25.00000000000000000, 347.0000000000000568, -59.99999999999999289 ) ) ;
#3559 = ORIENTED_EDGE ( 'NONE', *, *, #4758, .F. ) ;
#3560 = EDGE_CURVE ( 'NONE', #3822, #6450, #5960, .T. ) ;
#3561 =( LENGTH_UNIT ( ) NAMED_UNIT ( * ) SI_UNIT ( .MILLI., .METRE. ) );
#3562 = CARTESIAN_POINT ( 'NONE',  ( -20.00000000000000355, 63.00000000000000000, -57.08203932499370836 ) ) ;
#3563 = CARTESIAN_POINT ( 'NONE',  ( 0.000000000000000000, 265.0000000000000000, 95.00000000000002842 ) ) ;
#3564 = FACE_BOUND ( 'NONE', #7875, .T. ) ;
#3565 = ORIENTED_EDGE ( 'NONE', *, *, #4744, .T. ) ;
#3566 = CARTESIAN_POINT ( 'NONE',  ( 2.708734125000000326, 110.3124999986344079, 0.000000000000000000 ) ) ;
#3567 = DIRECTION ( 'NONE',  ( 0.000000000000000000, -0.000000000000000000, -1.000000000000000000 ) ) ;
#3568 = EDGE_CURVE ( 'NONE', #950, #1278, #2207, .T. ) ;
#3569 = ORIENTED_EDGE ( 'NONE', *, *, #2183, .T. ) ;
#3570 = PLANE ( 'NONE',  #9533 ) ;
#3571 = CARTESIAN_POINT ( 'NONE',  ( 70.71657310242181893, 47.47535718540355987, 24.98455589012892375 ) ) ;
#3572 = ORIENTED_EDGE ( 'NONE', *, *, #5190, .T. ) ;
#3573 = DIRECTION ( 'NONE',  ( -0.4999999999999942268, 0.8660254037844419273, 0.000000000000000000 ) ) ;
#3574 = DIRECTION ( 'NONE',  ( 0.000000000000000000, 1.000000000000000000, 0.000000000000000000 ) ) ;
#3575 = VERTEX_POINT ( 'NONE', #1962 ) ;
#3576 = DIRECTION ( 'NONE',  ( -0.000000000000000000, -1.000000000000000000, -0.000000000000000000 ) ) ;
#3577 = CARTESIAN_POINT ( 'NONE',  ( -5.974274778359173865, 21.21474596215567487, 80.00000000000000000 ) ) ;
#3578 = DIRECTION ( 'NONE',  ( 0.000000000000000000, 0.000000000000000000, 1.000000000000000000 ) ) ;
#3579 = CIRCLE ( 'NONE', #6360, 100.0000000000000142 ) ;
#3580 = CIRCLE ( 'NONE', #2581, 90.00000000000002842 ) ;
#3581 = CARTESIAN_POINT ( 'NONE',  ( -1.121994411437818862, 111.8749999986343937, 2.708734124999999882 ) ) ;
#3582 = EDGE_CURVE ( 'NONE', #4047, #1244, #9802, .T. ) ;
#3583 = EDGE_LOOP ( 'NONE', ( #7601, #7714, #3152, #7925 ) ) ;
#3584 = VECTOR ( 'NONE', #4173, 1000.000000000000000 ) ;
#3585 = CARTESIAN_POINT ( 'NONE',  ( 0.2500000000000002220, 4.898587196589412829E-16, -4.000000000000000000 ) ) ;
#3586 = LINE ( 'NONE', #1837, #2751 ) ;
#3587 = CARTESIAN_POINT ( 'NONE',  ( 117.9289321881355193, 50.00000000000008527, 25.00000000000000000 ) ) ;
#3588 = ADVANCED_FACE ( 'NONE', ( #5327 ), #9193, .F. ) ;
#3589 = LINE ( 'NONE', #4458, #8976 ) ;
#3590 = CARTESIAN_POINT ( 'NONE',  ( 109.9268209223821628, 285.0000000000000568, 32.26598893414752212 ) ) ;
#3591 = PLANE ( 'NONE',  #11484 ) ;
#3592 = LINE ( 'NONE', #1417, #11388 ) ;
#3593 = CARTESIAN_POINT ( 'NONE',  ( 3.250000000000000444, 111.0625000000000000, 1.346194077712559389 ) ) ;
#3594 = AXIS2_PLACEMENT_3D ( 'NONE', #6723, #4158, #2290 ) ;
#3595 = CARTESIAN_POINT ( 'NONE',  ( 0.000000000000000000, 216.0365690573663926, 0.000000000000000000 ) ) ;
#3596 = AXIS2_PLACEMENT_3D ( 'NONE', #5590, #1904, #4835 ) ;
#3597 = DIRECTION ( 'NONE',  ( 0.8660254037844397068, 0.4999999999999981681, 0.000000000000000000 ) ) ;
#3598 = ORIENTED_EDGE ( 'NONE', *, *, #6620, .T. ) ;
#3599 = AXIS2_PLACEMENT_3D ( 'NONE', #10549, #2253, #9668 ) ;
#3600 = DIRECTION ( 'NONE',  ( 0.000000000000000000, -0.5000000000000009992, -0.8660254037844380415 ) ) ;
#3601 = EDGE_CURVE ( 'NONE', #5901, #950, #9655, .T. ) ;
#3602 = DIRECTION ( 'NONE',  ( 0.000000000000000000, 0.000000000000000000, 1.000000000000000000 ) ) ;
#3603 = EDGE_CURVE ( 'NONE', #11761, #12227, #12248, .T. ) ;
#3604 = DIRECTION ( 'NONE',  ( 0.000000000000000000, 0.000000000000000000, -1.000000000000000000 ) ) ;
#3605 = ORIENTED_EDGE ( 'NONE', *, *, #584, .T. ) ;
#3606 = CARTESIAN_POINT ( 'NONE',  ( 63.96446609406733330, -63.96446609406769568, -20.00000000000000000 ) ) ;
#3607 = DIRECTION ( 'NONE',  ( -1.000000000000000000, -0.000000000000000000, -0.000000000000000000 ) ) ;
#3608 = CIRCLE ( 'NONE', #2814, 45.00000000000000000 ) ;
#3609 = EDGE_CURVE ( 'NONE', #4534, #4062, #5705, .T. ) ;
#3610 = ORIENTED_EDGE ( 'NONE', *, *, #11582, .F. ) ;
#3611 = LINE ( 'NONE', #9204, #4174 ) ;
#3612 = VECTOR ( 'NONE', #11722, 1000.000000000000000 ) ;
#3613 = ORIENTED_EDGE ( 'NONE', *, *, #1071, .T. ) ;
#3614 = AXIS2_PLACEMENT_3D ( 'NONE', #345, #8069, #409 ) ;
#3615 = CARTESIAN_POINT ( 'NONE',  ( 0.000000000000000000, 285.0000000000000568, 0.000000000000000000 ) ) ;
#3617 = ORIENTED_EDGE ( 'NONE', *, *, #2595, .T. ) ;
#3616 = CARTESIAN_POINT ( 'NONE',  ( 30.43816488677641985, 80.28464834591375165, -2.971076217724743618 ) ) ;
#3618 = ORIENTED_EDGE ( 'NONE', *, *, #7585, .F. ) ;
#3619 = CARTESIAN_POINT ( 'NONE',  ( 3.592712519748626931, 21.21474596215575659, 79.50000000000000000 ) ) ;
#3620 = FACE_OUTER_BOUND ( 'NONE', #7230, .T. ) ;
#3621 = AXIS2_PLACEMENT_3D ( 'NONE', #8657, #7668, #10531 ) ;
#3622 = VERTEX_POINT ( 'NONE', #8240 ) ;
#3623 = DIRECTION ( 'NONE',  ( 0.000000000000000000, -1.000000000000000000, 0.000000000000000000 ) ) ;
#3624 = CARTESIAN_POINT ( 'NONE',  ( 8.572527594031472993E-15, 63.00000000000000000, -70.00000000000000000 ) ) ;
#3625 = FACE_OUTER_BOUND ( 'NONE', #10039, .T. ) ;
#3626 = ORIENTED_EDGE ( 'NONE', *, *, #901, .T. ) ;
#3627 = CARTESIAN_POINT ( 'NONE',  ( -2.708734124999999882, 112.0624999986344079, 3.317242575922456639E-16 ) ) ;
#3628 = LINE ( 'NONE', #9160, #4005 ) ;
#3629 = ORIENTED_EDGE ( 'NONE', *, *, #11692, .F. ) ;
#3630 = EDGE_CURVE ( 'NONE', #834, #8527, #5778, .T. ) ;
#3631 = DIRECTION ( 'NONE',  ( 0.000000000000000000, 0.000000000000000000, 1.000000000000000000 ) ) ;
#3632 = DIRECTION ( 'NONE',  ( -1.000000000000000000, -0.000000000000000000, -0.000000000000000000 ) ) ;
#3633 = ORIENTED_EDGE ( 'NONE', *, *, #559, .F. ) ;
#3634 = CARTESIAN_POINT ( 'NONE',  ( 9.184850993605150311E-15, 10.00000000000017586, 75.00000000000001421 ) ) ;
#3635 = DIRECTION ( 'NONE',  ( 0.000000000000000000, 0.000000000000000000, 1.000000000000000000 ) ) ;
#3636 = ORIENTED_EDGE ( 'NONE', *, *, #8930, .T. ) ;
#3637 = DIRECTION ( 'NONE',  ( 0.000000000000000000, 0.000000000000000000, -1.000000000000000000 ) ) ;
#3638 = FACE_OUTER_BOUND ( 'NONE', #9661, .T. ) ;
#3639 = AXIS2_PLACEMENT_3D ( 'NONE', #11881, #10686, #7876 ) ;
#3640 = EDGE_CURVE ( 'NONE', #11487, #5761, #722, .T. ) ;
#3641 = CARTESIAN_POINT ( 'NONE',  ( -1.121994411437818862, 110.8749999986343937, 2.708734124999999882 ) ) ;
#3642 = CARTESIAN_POINT ( 'NONE',  ( -1.915364268218908927, 110.9374999986344079, 1.915364268218909150 ) ) ;
#3643 = VERTEX_POINT ( 'NONE', #4567 ) ;
#3644 = ORIENTED_EDGE ( 'NONE', *, *, #449, .F. ) ;
#3645 =( LENGTH_UNIT ( ) NAMED_UNIT ( * ) SI_UNIT ( .MILLI., .METRE. ) );
#3646 = VECTOR ( 'NONE', #5294, 1000.000000000000000 ) ;
#3647 = CARTESIAN_POINT ( 'NONE',  ( 0.000000000000000000, 265.0000000000000000, 0.000000000000000000 ) ) ;
#3648 = CARTESIAN_POINT ( 'NONE',  ( 11.80921887069467324, 30.25000000000018474, 79.50000000000000000 ) ) ;
#3649 = CARTESIAN_POINT ( 'NONE',  ( -25.00000000000000000, 445.0000000000000568, -31.99999999999999289 ) ) ;
#3650 = LINE ( 'NONE', #9247, #3024 ) ;
#3651 = ADVANCED_FACE ( 'NONE', ( #12125 ), #1827, .F. ) ;
#3652 = CARTESIAN_POINT ( 'NONE',  ( -27.54203853141981995, 86.50063778822037364, -11.90690952824024329 ) ) ;
#3653 = FACE_OUTER_BOUND ( 'NONE', #10442, .T. ) ;
#3654 = CARTESIAN_POINT ( 'NONE',  ( 5.092712519748611832, 18.61666975080242992, 79.50000000000000000 ) ) ;
#3655 = EDGE_CURVE ( 'NONE', #2607, #4918, #12061, .T. ) ;
#3656 = VECTOR ( 'NONE', #2850, 1000.000000000000114 ) ;
#3657 = CARTESIAN_POINT ( 'NONE',  ( 24.99999999999999645, 445.0000000000000568, -95.00000000000000000 ) ) ;
#3658 = B_SPLINE_CURVE_WITH_KNOTS ( 'NONE', 3,
 ( #5143, #4314, #10988, #2202, #6255, #8109, #8919, #2451, #7988, #11934, #3203, #9985, #7003, #10045, #6191, #451, #6012, #576 ),
 .UNSPECIFIED., .F., .F.,
 ( 4, 2, 2, 2, 2, 2, 2, 2, 4 ),
 ( 0.000000000000000000, 0.001070780962355597247, 0.002141561924711194494, 0.003212342887066791525, 0.004283123849422388989, 0.005353904811777986453, 0.006424685774133583049, 0.007495466736489180513, 0.008566247698844777977 ),
 .UNSPECIFIED. ) ;
#3659 = CARTESIAN_POINT ( 'NONE',  ( -7.474274778359198734, 41.38333024919781167, 80.00000000000000000 ) ) ;
#3660 = EDGE_LOOP ( 'NONE', ( #1072, #12123, #3182, #9979 ) ) ;
#3661 = EDGE_CURVE ( 'NONE', #9442, #10391, #1714, .T. ) ;
#3662 = EDGE_CURVE ( 'NONE', #10032, #8236, #5897, .T. ) ;
#3663 = DIRECTION ( 'NONE',  ( 0.000000000000000000, -1.000000000000000000, 0.000000000000000000 ) ) ;
#3664 = AXIS2_PLACEMENT_3D ( 'NONE', #3899, #11508, #2960 ) ;
#3665 = CIRCLE ( 'NONE', #10630, 8.000000000000000000 ) ;
#3666 = DIRECTION ( 'NONE',  ( 0.000000000000000000, 1.000000000000000000, 0.000000000000000000 ) ) ;
#3667 = CARTESIAN_POINT ( 'NONE',  ( 70.79098555896973721, 19.56855962084436129, -24.99999999902147962 ) ) ;
#3668 = ORIENTED_EDGE ( 'NONE', *, *, #9330, .F. ) ;
#3669 = DIRECTION ( 'NONE',  ( 0.000000000000000000, 0.000000000000000000, -1.000000000000000000 ) ) ;
#3670 = DIRECTION ( 'NONE',  ( -6.938893903907222067E-15, -1.000000000000000000, 0.000000000000000000 ) ) ;
#3671 = ORIENTED_EDGE ( 'NONE', *, *, #1063, .T. ) ;
#3672 = CARTESIAN_POINT ( 'NONE',  ( 147.9289321881356045, 20.00000000000009237, 25.00000000000000000 ) ) ;
#3673 = CIRCLE ( 'NONE', #1683, 25.00000000000000000 ) ;
#3674 = PRODUCT_DEFINITION ( 'UNKNOWN', '', #11531, #10743 ) ;
#3675 = ORIENTED_EDGE ( 'NONE', *, *, #9455, .F. ) ;
#3676 = CARTESIAN_POINT ( 'NONE',  ( 0.000000000000000000, 87.50000000000000000, 0.000000000000000000 ) ) ;
#3677 = DIRECTION ( 'NONE',  ( 0.000000000000000000, 0.000000000000000000, 1.000000000000000000 ) ) ;
#3678 = ORIENTED_EDGE ( 'NONE', *, *, #7495, .F. ) ;
#3679 = CARTESIAN_POINT ( 'NONE',  ( 2.500000000000000000, 2.357898499370431722, -2.818925648462311528E-15 ) ) ;
#3680 = VERTEX_POINT ( 'NONE', #10236 ) ;
#3681 = AXIS2_PLACEMENT_3D ( 'NONE', #3170, #2355, #6161 ) ;
#3682 = DIRECTION ( 'NONE',  ( 1.000000000000000000, 0.000000000000000000, 0.000000000000000000 ) ) ;
#3683 = DIRECTION ( 'NONE',  ( 0.000000000000000000, 1.000000000000000000, 0.000000000000000000 ) ) ;
#3684 = ORIENTED_EDGE ( 'NONE', *, *, #10831, .T. ) ;
#3685 = CARTESIAN_POINT ( 'NONE',  ( -2.708734124999999882, 111.0624999986344079, 3.317242575922456639E-16 ) ) ;
#3686 = FACE_OUTER_BOUND ( 'NONE', #10497, .T. ) ;
#3687 = ADVANCED_FACE ( 'NONE', ( #8422, #896 ), #3693, .T. ) ;
#3688 = CIRCLE ( 'NONE', #1106, 10.49999999999999822 ) ;
#3689 = ORIENTED_EDGE ( 'NONE', *, *, #9515, .F. ) ;
#3690 = CARTESIAN_POINT ( 'NONE',  ( -15.31872880306210583, 24.93376880718456334, 73.41908715900406435 ) ) ;
#3691 = EDGE_LOOP ( 'NONE', ( #9508, #12132, #4184, #10714 ) ) ;
#3692 = CARTESIAN_POINT ( 'NONE',  ( 13.80921887069452758, 30.00000000000009237, 65.00000000000000000 ) ) ;
#3693 = PLANE ( 'NONE',  #2112 ) ;
#3694 = ORIENTED_EDGE ( 'NONE', *, *, #5318, .F. ) ;
#3695 = LINE ( 'NONE', #6513, #8088 ) ;
#3696 = DIRECTION ( 'NONE',  ( 3.469446951953613203E-16, -0.000000000000000000, 1.000000000000000000 ) ) ;
#3697 = VECTOR ( 'NONE', #7382, 1000.000000000000000 ) ;
#3698 = CARTESIAN_POINT ( 'NONE',  ( -2.298097038856279806, 114.4999999972688158, -2.298097038856279362 ) ) ;
#3699 = CARTESIAN_POINT ( 'NONE',  ( -2.708734124999999882, 110.9999999986343937, 1.121994411437819084 ) ) ;
#3700 = ORIENTED_EDGE ( 'NONE', *, *, #1773, .T. ) ;
#3701 =( NAMED_UNIT ( * ) SI_UNIT ( $, .STERADIAN. ) SOLID_ANGLE_UNIT ( ) );
#3702 = TOROIDAL_SURFACE ( 'NONE', #10668, 10.00000000000000000, 5.000000000000000000 ) ;
#3703 = EDGE_CURVE ( 'NONE', #4222, #11096, #2756, .T. ) ;
#3704 = CARTESIAN_POINT ( 'NONE',  ( 0.000000000000000000, 265.0000000000000000, 0.000000000000000000 ) ) ;
#3705 = EDGE_CURVE ( 'NONE', #938, #7550, #2575, .T. ) ;
#3706 = CARTESIAN_POINT ( 'NONE',  ( 63.96446609406734751, -63.96446609406770989, -25.00000000000000000 ) ) ;
#3707 = ORIENTED_EDGE ( 'NONE', *, *, #8169, .F. ) ;
#3708 = CARTESIAN_POINT ( 'NONE',  ( -0.9407811293052825707, 17.00000000000008882, 80.00000000000000000 ) ) ;
#3709 = CARTESIAN_POINT ( 'NONE',  ( -25.00000000000000000, 445.0000000000000568, -14.99999999999999289 ) ) ;
#3710 = PRESENTATION_LAYER_ASSIGNMENT (  '', '', ( #11886 ) ) ;
#3711 = LINE ( 'NONE', #6336, #11290 ) ;
#3712 = DIRECTION ( 'NONE',  ( 0.000000000000000000, 0.000000000000000000, 1.000000000000000000 ) ) ;
#3713 = SHAPE_REPRESENTATION ( 'BR-821', ( #9919, #9111, #1371, #5950, #11932, #5756, #1570, #9317, #8325 ), #7144 ) ;
#3714 = ORIENTED_EDGE ( 'NONE', *, *, #348, .T. ) ;
#3715 = PLANE ( 'NONE',  #606 ) ;
#3716 = VECTOR ( 'NONE', #4447, 1000.000000000000000 ) ;
#3717 = EDGE_CURVE ( 'NONE', #6916, #5925, #5452, .T. ) ;
#3718 = ADVANCED_FACE ( 'NONE', ( #1077 ), #4753, .T. ) ;
#3719 = DIRECTION ( 'NONE',  ( 1.000000000000000000, -0.000000000000000000, 1.224646799147353207E-16 ) ) ;
#3720 = DIRECTION ( 'NONE',  ( -1.000000000000000000, 0.000000000000000000, 0.000000000000000000 ) ) ;
#3721 = ORIENTED_EDGE ( 'NONE', *, *, #2123, .T. ) ;
#3722 = PLANE ( 'NONE',  #7832 ) ;
#3723 = CARTESIAN_POINT ( 'NONE',  ( 0.000000000000000000, 110.0000000000000000, 3.250000000000000444 ) ) ;
#3724 = CARTESIAN_POINT ( 'NONE',  ( -1.440781129305282571, 17.00000000000009592, 79.50000000000000000 ) ) ;
#3725 = ORIENTED_EDGE ( 'NONE', *, *, #11408, .F. ) ;
#3726 = DIRECTION ( 'NONE',  ( -0.000000000000000000, 1.000000000000000000, -0.000000000000000000 ) ) ;
#3727 = DIRECTION ( 'NONE',  ( 0.000000000000000000, 0.000000000000000000, 1.000000000000000000 ) ) ;
#3728 = VERTEX_POINT ( 'NONE', #7681 ) ;
#3729 = CARTESIAN_POINT ( 'NONE',  ( -25.00000000000000000, 445.0000000000000568, -29.99999999999999289 ) ) ;
#3730 = B_SPLINE_CURVE_WITH_KNOTS ( 'NONE', 3,
 ( #8145, #2486, #6350, #1428, #6227, #9894, #8022, #10898, #3234, #3483, #11968, #10137, #7100, #6290, #11022, #5234, #10078, #11849 ),
 .UNSPECIFIED., .F., .F.,
 ( 4, 2, 2, 2, 2, 2, 2, 2, 4 ),
 ( 0.000000000000000000, 0.001070893387785249720, 0.002141786775570499440, 0.003212680163355748943, 0.004283573551140998879, 0.005354466938926247949, 0.006425360326711500487, 0.007496253714496753026, 0.008567147102282004698 ),
 .UNSPECIFIED. ) ;
#3731 = ADVANCED_FACE ( 'NONE', ( #9479 ), #3068, .F. ) ;
#3732 = EDGE_LOOP ( 'NONE', ( #145, #8543 ) ) ;
#3733 = DIRECTION ( 'NONE',  ( 0.8660254037844331565, -0.5000000000000095479, 0.000000000000000000 ) ) ;
#3734 = DIRECTION ( 'NONE',  ( -0.000000000000000000, -1.000000000000000000, -0.000000000000000000 ) ) ;
#3735 = VERTEX_POINT ( 'NONE', #4885 ) ;
#3736 = DIRECTION ( 'NONE',  ( -0.000000000000000000, 0.8660254037844402619, -0.4999999999999975575 ) ) ;
#3737 = EDGE_LOOP ( 'NONE', ( #9152, #11526 ) ) ;
#3738 = DIRECTION ( 'NONE',  ( 0.000000000000000000, 0.000000000000000000, 1.000000000000000000 ) ) ;
#3739 = CARTESIAN_POINT ( 'NONE',  ( 5.525725221640672480, 41.13333024919784719, 80.00000000000000000 ) ) ;
#3740 = DIRECTION ( 'NONE',  ( -0.000000000000000000, -1.000000000000000000, -0.000000000000000000 ) ) ;
#3741 = DIRECTION ( 'NONE',  ( -0.000000000000000000, -1.000000000000000000, -0.000000000000000000 ) ) ;
#3742 = VECTOR ( 'NONE', #5617, 1000.000000000000000 ) ;
#3743 = PRESENTATION_LAYER_ASSIGNMENT (  '', '', ( #5155 ) ) ;
#3744 = VERTEX_POINT ( 'NONE', #8669 ) ;
#3745 = CARTESIAN_POINT ( 'NONE',  ( 1.121994411437818862, 113.7499999986343937, 2.708734124999999882 ) ) ;
#3746 = LINE ( 'NONE', #7496, #1416 ) ;
#3747 = EDGE_LOOP ( 'NONE', ( #6322, #10090, #5519, #9965, #4660 ) ) ;
#3748 = AXIS2_PLACEMENT_3D ( 'NONE', #11196, #849, #8434 ) ;
#3749 = LINE ( 'NONE', #11551, #6762 ) ;
#3750 = PRODUCT_DEFINITION_FORMATION_WITH_SPECIFIED_SOURCE ( 'ANY', '', #102, .NOT_KNOWN. ) ;
#3751 = FACE_OUTER_BOUND ( 'NONE', #9923, .T. ) ;
#3752 = ORIENTED_EDGE ( 'NONE', *, *, #9309, .F. ) ;
#3753 = CARTESIAN_POINT ( 'NONE',  ( -2.298097038856279362, 112.3750000000000000, 2.298097038856279806 ) ) ;
#3754 = DIRECTION ( 'NONE',  ( 0.000000000000000000, -0.8660254037844402619, -0.4999999999999975575 ) ) ;
#3755 = VERTEX_POINT ( 'NONE', #8791 ) ;
#3756 = EDGE_CURVE ( 'NONE', #10965, #10533, #5107, .T. ) ;
#3757 = EDGE_CURVE ( 'NONE', #10391, #8715, #11496, .T. ) ;
#3758 = DIRECTION ( 'NONE',  ( 0.000000000000000000, 0.000000000000000000, 1.000000000000000000 ) ) ;
#3759 = LINE ( 'NONE', #2885, #4594 ) ;
#3760 = CARTESIAN_POINT ( 'NONE',  ( 1.121994411437818862, 112.7499999986343937, 2.708734124999999882 ) ) ;
#3761 = CARTESIAN_POINT ( 'NONE',  ( -32.05000697088088657, 85.26794919243110371, -9.660254037844429931 ) ) ;
#3762 = EDGE_CURVE ( 'NONE', #12030, #1340, #3944, .T. ) ;
#3763 = ORIENTED_EDGE ( 'NONE', *, *, #8591, .T. ) ;
#3764 = ORIENTED_EDGE ( 'NONE', *, *, #3131, .T. ) ;
#3765 = VECTOR ( 'NONE', #10694, 1000.000000000000000 ) ;
#3766 = DIRECTION ( 'NONE',  ( -0.8660254037844377084, 0.5000000000000015543, 0.000000000000000000 ) ) ;
#3767 = CARTESIAN_POINT ( 'NONE',  ( 2.500000000000000000, 0.000000000000000000, 0.000000000000000000 ) ) ;
#3768 = VERTEX_POINT ( 'NONE', #11620 ) ;
#3769 = DIRECTION ( 'NONE',  ( 0.000000000000000000, 1.000000000000000000, 0.000000000000000000 ) ) ;
#3770 = CIRCLE ( 'NONE', #6956, 2.649999999999987477 ) ;
#3771 = VECTOR ( 'NONE', #10483, 1000.000000000000114 ) ;
#3772 = CARTESIAN_POINT ( 'NONE',  ( 0.000000000000000000, -10.00000000000000000, 0.000000000000000000 ) ) ;
#3773 = CARTESIAN_POINT ( 'NONE',  ( 1.285879139104721264E-14, 260.0000000000000000, -105.0000000000000426 ) ) ;
#3774 = DIRECTION ( 'NONE',  ( -0.8660254037844394848, -0.4999999999999985567, 0.000000000000000000 ) ) ;
#3775 = AXIS2_PLACEMENT_3D ( 'NONE', #8335, #2670, #10396 ) ;
#3776 = AXIS2_PLACEMENT_3D ( 'NONE', #10386, #2848, #2911 ) ;
#3777 = UNCERTAINTY_MEASURE_WITH_UNIT (LENGTH_MEASURE( 1.000000000000000082E-05 ), #3645, 'distance_accuracy_value', 'NONE');
#3778 = CARTESIAN_POINT ( 'NONE',  ( 69.52686081652184669, 40.00000000000008527, -28.12500000000000000 ) ) ;
#3779 = AXIS2_PLACEMENT_3D ( 'NONE', #2141, #6631, #1025 ) ;
#3780 = FILL_AREA_STYLE ('',( #10448 ) ) ;
#3781 = EDGE_LOOP ( 'NONE', ( #6244, #3855, #10418, #12312 ) ) ;
#3782 = EDGE_CURVE ( 'NONE', #4212, #10619, #512, .T. ) ;
#3783 = CARTESIAN_POINT ( 'NONE',  ( 27.96741528345890870, 86.27927944434865992, 11.41192941739706335 ) ) ;
#3784 =( BOUNDED_CURVE ( )  B_SPLINE_CURVE ( 2, ( #10690, #7822, #8872, #340, #11760, #3212, #1099, #2093, #4206, #6765, #2034, #5839, #8691, #3964, #5900, #9683, #1160, #4963, #10998, #6263, #8058, #4384, #11884, #11825, #11063, #7074, #1528, #2525, #2460, #10175, #7996, #525, #11125, #2333, #1587, #11941, #10053, #6325, #1466, #5331, #12066, #9108, #4322, #2392, #3336, #3460, #586, #7134, #3523, #9236, #8182, #5272, #12005, #7262, #3267, #10875, #10109, #5392, #5211, #10931, #9172, #653, #7326, #6141, #2579 ),
 .UNSPECIFIED., .F., .F. ) 
 B_SPLINE_CURVE_WITH_KNOTS ( ( 3, 2, 2, 2, 2, 2, 2, 2, 2, 2, 2, 2, 2, 2, 2, 2, 2, 2, 2, 2, 2, 2, 2, 2, 2, 2, 2, 2, 2, 2, 2, 2, 3 ),
 ( 0.000000000000000000, 0.03125000000000000000, 0.06250000000000000000, 0.09375000000000000000, 0.1250000000000000000, 0.1562500000000000000, 0.1875000000000000000, 0.2187500000000000000, 0.2500000000000000000, 0.2812500000000000000, 0.3125000000000000000, 0.3437500000000000000, 0.3750000000000000000, 0.4062500000000000000, 0.4375000000000000000, 0.4687500000000000000, 0.5000000000000000000, 0.5312500000000000000, 0.5625000000000000000, 0.5937500000000000000, 0.6250000000000000000, 0.6562500000000000000, 0.6875000000000000000, 0.7187500000000000000, 0.7500000000000000000, 0.7812500000000000000, 0.8125000000000000000, 0.8437500000000000000, 0.8750000000000000000, 0.9062500000000000000, 0.9375000000000000000, 0.9687500000000000000, 1.000000000000000000 ),
 .UNSPECIFIED. ) 
 CURVE ( )  GEOMETRIC_REPRESENTATION_ITEM ( )  RATIONAL_B_SPLINE_CURVE ( ( 1.000000000000000000, 0.9238795325112867385, 1.000000000000000000, 0.9238795325112867385, 1.000000000000000000, 0.9238795325112867385, 1.000000000000000000, 0.9238795325112867385, 1.000000000000000000, 0.9238795325112867385, 1.000000000000000000, 0.9238795325112867385, 1.000000000000000000, 0.9238795325112867385, 1.000000000000000000, 0.9238795325112867385, 1.000000000000000000, 0.9238795325112867385, 1.000000000000000000, 0.9238795325112867385, 1.000000000000000000, 0.9238795325112867385, 1.000000000000000000, 0.9238795325112867385, 1.000000000000000000, 0.9238795325112867385, 1.000000000000000000, 0.9238795325112867385, 1.000000000000000000, 0.9238795325112867385, 1.000000000000000000, 0.9238795325112867385, 1.000000000000000000, 0.9238795325112867385, 1.000000000000000000, 0.9238795325112867385, 1.000000000000000000, 0.9238795325112867385, 1.000000000000000000, 0.9238795325112867385, 1.000000000000000000, 0.9238795325112867385, 1.000000000000000000, 0.9238795325112867385, 1.000000000000000000, 0.9238795325112867385, 1.000000000000000000, 0.9238795325112867385, 1.000000000000000000, 0.9238795325112867385, 1.000000000000000000, 0.9238795325112867385, 1.000000000000000000, 0.9238795325112867385, 1.000000000000000000, 0.9238795325112867385, 1.000000000000000000, 0.9238795325112867385, 1.000000000000000000, 0.9238795325112867385, 1.000000000000000000, 0.9238795325112867385, 1.000000000000000000, 0.9238795325112867385, 1.000000000000000000 ) ) 
 REPRESENTATION_ITEM ( '' )  );
#3785 = CARTESIAN_POINT ( 'NONE',  ( 0.000000000000000000, 165.0000000000000000, 0.000000000000000000 ) ) ;
#3786 = CARTESIAN_POINT ( 'NONE',  ( 69.55283199277543815, 18.65681359763190628, -28.06103394134222029 ) ) ;
#3787 = ORIENTED_EDGE ( 'NONE', *, *, #91, .T. ) ;
#3788 = CIRCLE ( 'NONE', #5594, 2.500000000000000888 ) ;
#3789 = CARTESIAN_POINT ( 'NONE',  ( 135.0000000000011084, 67.07106781186550393, -19.99999999999999645 ) ) ;
#3790 = PRODUCT_DEFINITION_SHAPE ( 'NONE', 'NONE',  #11834 ) ;
#3791 = CARTESIAN_POINT ( 'NONE',  ( -1.190781129305471087, 30.00000000000008882, 80.00000000000000000 ) ) ;
#3792 = ADVANCED_FACE ( 'NONE', ( #10728 ), #6748, .F. ) ;
#3793 = EDGE_LOOP ( 'NONE', ( #2895, #3636 ) ) ;
#3794 = DIRECTION ( 'NONE',  ( 0.000000000000000000, 1.000000000000000000, 0.000000000000000000 ) ) ;
#3795 = VECTOR ( 'NONE', #2078, 1000.000000000000000 ) ;
#3796 =( GEOMETRIC_REPRESENTATION_CONTEXT ( 3 ) GLOBAL_UNCERTAINTY_ASSIGNED_CONTEXT ( ( #6268 ) ) GLOBAL_UNIT_ASSIGNED_CONTEXT ( ( #10444, #2155, #1910 ) ) REPRESENTATION_CONTEXT ( 'NONE', 'WORKASPACE' ) );
#3797 = VERTEX_POINT ( 'NONE', #10607 ) ;
#3798 = LINE ( 'NONE', #7599, #1561 ) ;
#3799 = CARTESIAN_POINT ( 'NONE',  ( 28.72281323269012532, 77.00000000000000000, -8.660254037844445918 ) ) ;
#3800 = ORIENTED_EDGE ( 'NONE', *, *, #973, .T. ) ;
#3801 = FACE_OUTER_BOUND ( 'NONE', #11494, .T. ) ;
#3802 = CARTESIAN_POINT ( 'NONE',  ( 2.500000000000000000, -1.178949249685214307, 2.042000000000001592 ) ) ;
#3803 = ORIENTED_EDGE ( 'NONE', *, *, #7194, .F. ) ;
#3804 = ADVANCED_FACE ( 'NONE', ( #2072 ), #6, .F. ) ;
#3805 = EDGE_CURVE ( 'NONE', #9112, #1236, #2136, .T. ) ;
#3806 = CARTESIAN_POINT ( 'NONE',  ( 0.000000000000000000, 115.0000000000000000, 0.000000000000000000 ) ) ;
#3808 = DIRECTION ( 'NONE',  ( 0.000000000000000000, 0.000000000000000000, -1.000000000000000000 ) ) ;
#3807 = AXIS2_PLACEMENT_3D ( 'NONE', #4933, #120, #4056 ) ;
#3809 = DIRECTION ( 'NONE',  ( -1.000000000000000000, 0.000000000000000000, -6.938893903907222461E-16 ) ) ;
#3810 = ORIENTED_EDGE ( 'NONE', *, *, #6550, .F. ) ;
#3811 = CARTESIAN_POINT ( 'NONE',  ( -1.915364268218908927, 112.9374999986344079, 1.915364268218909150 ) ) ;
#3812 = CARTESIAN_POINT ( 'NONE',  ( 1.346194077712559389, 113.0624999972688016, 3.250000000000000444 ) ) ;
#3813 = AXIS2_PLACEMENT_3D ( 'NONE', #12043, #6493, #691 ) ;
#3814 = ADVANCED_FACE ( 'NONE', ( #4944 ), #10545, .T. ) ;
#3815 = CIRCLE ( 'NONE', #1228, 5.000000000000000888 ) ;
#3816 = ORIENTED_EDGE ( 'NONE', *, *, #4910, .T. ) ;
#3817 = DIRECTION ( 'NONE',  ( 0.000000000000000000, 1.000000000000000000, 0.000000000000000000 ) ) ;
#3818 = CARTESIAN_POINT ( 'NONE',  ( 69.55111042745878080, 41.29936696797726370, 28.06526308249823032 ) ) ;
#3819 = ORIENTED_EDGE ( 'NONE', *, *, #10882, .T. ) ;
#3820 = LINE ( 'NONE', #9413, #12037 ) ;
#3821 = DIRECTION ( 'NONE',  ( 0.8660254037844331565, -0.5000000000000095479, 0.000000000000000000 ) ) ;
#3822 = VERTEX_POINT ( 'NONE', #1949 ) ;
#3823 = EDGE_CURVE ( 'NONE', #8953, #7769, #5760, .T. ) ;
#3824 = CARTESIAN_POINT ( 'NONE',  ( -14.19078112930533209, 29.75000000000008882, 79.50000000000000000 ) ) ;
#3825 = DIRECTION ( 'NONE',  ( -0.000000000000000000, -0.000000000000000000, 1.000000000000000000 ) ) ;
#3826 = APPLICATION_CONTEXT ( 'automotive_design' ) ;
#3827 = CARTESIAN_POINT ( 'NONE',  ( 25.00000000000000000, 445.0000000000000568, -24.99999999999998934 ) ) ;
#3828 = CARTESIAN_POINT ( 'NONE',  ( 142.0710678118665555, 59.99999999999998579, 25.00000000000000000 ) ) ;
#3829 = CARTESIAN_POINT ( 'NONE',  ( -1.121994411437820194, 112.2499999986343937, -2.708734124999999437 ) ) ;
#3830 = ORIENTED_EDGE ( 'NONE', *, *, #5344, .F. ) ;
#3831 = EDGE_CURVE ( 'NONE', #6555, #8595, #11016, .T. ) ;
#3832 = ORIENTED_EDGE ( 'NONE', *, *, #6310, .T. ) ;
#3833 = ADVANCED_FACE ( 'NONE', ( #3314 ), #440, .F. ) ;
#3834 = SURFACE_STYLE_FILL_AREA ( #11446 ) ;
#3835 = DIRECTION ( 'NONE',  ( 1.000000000000000000, -1.040834085586083310E-14, 0.000000000000000000 ) ) ;
#3836 = AXIS2_PLACEMENT_3D ( 'NONE', #9245, #731, #12012 ) ;
#3837 = ORIENTED_EDGE ( 'NONE', *, *, #7456, .T. ) ;
#3838 = PLANE ( 'NONE',  #8002 ) ;
#3839 = DIRECTION ( 'NONE',  ( 0.000000000000000000, 0.000000000000000000, 1.000000000000000000 ) ) ;
#3840 = CARTESIAN_POINT ( 'NONE',  ( -31.68100721119781937, 75.82462385531685811, 6.696065238440062295 ) ) ;
#3841 = CARTESIAN_POINT ( 'NONE',  ( -5.999999999999999112, 62.00000000000000000, 60.00000000000002132 ) ) ;
#3842 = ORIENTED_EDGE ( 'NONE', *, *, #3284, .T. ) ;
#3843 = VECTOR ( 'NONE', #3734, 1000.000000000000000 ) ;
#3844 = EDGE_CURVE ( 'NONE', #4861, #4898, #7974, .T. ) ;
#3845 = CARTESIAN_POINT ( 'NONE',  ( 0.000000000000000000, 265.0000000000000000, 100.0000000000000284 ) ) ;
#3846 = DIRECTION ( 'NONE',  ( 0.000000000000000000, 0.000000000000000000, -1.000000000000000000 ) ) ;
#3847 = CARTESIAN_POINT ( 'NONE',  ( -25.00000000000000000, 445.0000000000000568, -59.99999999999999289 ) ) ;
#3848 = FACE_OUTER_BOUND ( 'NONE', #11983, .T. ) ;
#3849 = LINE ( 'NONE', #6717, #2102 ) ;
#3850 = CARTESIAN_POINT ( 'NONE',  ( 71.45054378765421177, 15.85863886173339665, -22.96278406504537628 ) ) ;
#3851 = ORIENTED_EDGE ( 'NONE', *, *, #8061, .F. ) ;
#3852 = AXIS2_PLACEMENT_3D ( 'NONE', #3157, #344, #11006 ) ;
#3853 = CARTESIAN_POINT ( 'NONE',  ( 0.000000000000000000, 110.0000000000000000, 3.250000000000000444 ) ) ;
#3854 = DIRECTION ( 'NONE',  ( 0.000000000000000000, 0.000000000000000000, 1.000000000000000000 ) ) ;
#3855 = ORIENTED_EDGE ( 'NONE', *, *, #2305, .F. ) ;
#3856 = CARTESIAN_POINT ( 'NONE',  ( 9.942549119892413856, 23.28349364905404428, 80.00000000000000000 ) ) ;
#3857 = AXIS2_PLACEMENT_3D ( 'NONE', #9488, #972, #4762 ) ;
#3858 = CIRCLE ( 'NONE', #3491, 100.0000000000000284 ) ;
#3859 = ORIENTED_EDGE ( 'NONE', *, *, #2409, .T. ) ;
#3860 = ADVANCED_FACE ( 'NONE', ( #5071 ), #8848, .F. ) ;
#3861 = DIRECTION ( 'NONE',  ( -0.4999999999999985567, 0.8660254037844394848, 0.000000000000000000 ) ) ;
#3862 = DIRECTION ( 'NONE',  ( 0.000000000000000000, 0.000000000000000000, 1.000000000000000000 ) ) ;
#3863 = ORIENTED_EDGE ( 'NONE', *, *, #9304, .F. ) ;
#3864 = EDGE_CURVE ( 'NONE', #1669, #2064, #6492, .T. ) ;
#3865 = CARTESIAN_POINT ( 'NONE',  ( 30.23169114332096896, 76.99999999999998579, -5.192055827170280580 ) ) ;
#3866 = DIRECTION ( 'NONE',  ( 0.000000000000000000, 0.000000000000000000, 1.000000000000000000 ) ) ;
#3867 = ORIENTED_EDGE ( 'NONE', *, *, #6315, .T. ) ;
#3868 = CARTESIAN_POINT ( 'NONE',  ( 0.000000000000000000, 115.0000000000000000, 0.000000000000000000 ) ) ;
#3869 = CARTESIAN_POINT ( 'NONE',  ( -0.9407811293054709756, 40.00000000000008527, 80.00000000000000000 ) ) ;
#3870 = DIRECTION ( 'NONE',  ( 0.000000000000000000, -0.000000000000000000, 1.000000000000000000 ) ) ;
#3871 = AXIS2_PLACEMENT_3D ( 'NONE', #2822, #9478, #9293 ) ;
#3872 = EDGE_LOOP ( 'NONE', ( #3252, #8206, #4079, #10496 ) ) ;
#3873 = CARTESIAN_POINT ( 'NONE',  ( 1.915364268218908927, 114.1874999986344079, -1.915364268218909816 ) ) ;
#3874 = AXIS2_PLACEMENT_3D ( 'NONE', #809, #7416, #11218 ) ;
#3875 = PLANE ( 'NONE',  #9514 ) ;
#3876 = ORIENTED_EDGE ( 'NONE', *, *, #11312, .F. ) ;
#3877 = EDGE_CURVE ( 'NONE', #1231, #8595, #7485, .T. ) ;
#3878 = DIRECTION ( 'NONE',  ( -1.000000000000000000, 0.000000000000000000, 0.000000000000000000 ) ) ;
#3879 = CARTESIAN_POINT ( 'NONE',  ( -6.601480288436279764, 16.00045772279125700, 74.71048470746850967 ) ) ;
#3880 = AXIS2_PLACEMENT_3D ( 'NONE', #8204, #8144, #5420 ) ;
#3881 = VERTEX_POINT ( 'NONE', #9909 ) ;
#3882 = CIRCLE ( 'NONE', #1696, 12.99999999999999822 ) ;
#3883 = DIRECTION ( 'NONE',  ( 0.000000000000000000, 0.000000000000000000, -1.000000000000000000 ) ) ;
#3884 = CARTESIAN_POINT ( 'NONE',  ( 69.52686081652184669, 20.00000000000009237, 28.12499999999999645 ) ) ;
#3885 = ORIENTED_EDGE ( 'NONE', *, *, #2062, .F. ) ;
#3886 = CARTESIAN_POINT ( 'NONE',  ( -8.000000000000000000, 165.0000000000000000, -5.999999999999998224 ) ) ;
#3887 = EDGE_CURVE ( 'NONE', #3680, #4313, #2371, .T. ) ;
#3888 = CYLINDRICAL_SURFACE ( 'NONE', #125, 30.00000000000000711 ) ;
#3889 = DIRECTION ( 'NONE',  ( -0.000000000000000000, -0.000000000000000000, 1.000000000000000000 ) ) ;
#3890 = CARTESIAN_POINT ( 'NONE',  ( -27.96741528345882344, 86.27927944434871677, -11.41192941739715927 ) ) ;
#3891 = CARTESIAN_POINT ( 'NONE',  ( 3.249999999999999556, 112.9375000000000000, -1.346194077712561610 ) ) ;
#3892 = CARTESIAN_POINT ( 'NONE',  ( 72.45695464226038496, 14.86571900151108494, 19.37542581275875619 ) ) ;
#3893 = AXIS2_PLACEMENT_3D ( 'NONE', #1145, #10609, #1782 ) ;
#3894 = EDGE_LOOP ( 'NONE', ( #4612, #6603, #3763, #8179, #7992 ) ) ;
#3895 =( NAMED_UNIT ( * ) PLANE_ANGLE_UNIT ( ) SI_UNIT ( $, .RADIAN. ) );
#3896 = VECTOR ( 'NONE', #6432, 1000.000000000000000 ) ;
#3897 = ADVANCED_FACE ( 'NONE', ( #8035 ), #317, .T. ) ;
#3898 = EDGE_LOOP ( 'NONE', ( #3787, #7824, #11739, #170 ) ) ;
#3899 = CARTESIAN_POINT ( 'NONE',  ( 74.16198487095665826, 50.00000000000000000, 30.00000000000000355 ) ) ;
#3900 = CARTESIAN_POINT ( 'NONE',  ( 12.41779361890942290, 36.32650217634261480, 73.96515157582260258 ) ) ;
#3901 = ORIENTED_EDGE ( 'NONE', *, *, #11948, .F. ) ;
#3902 = FACE_OUTER_BOUND ( 'NONE', #3747, .T. ) ;
#3903 = AXIS2_PLACEMENT_3D ( 'NONE', #1201, #7741, #11555 ) ;
#3904 = CARTESIAN_POINT ( 'NONE',  ( 0.000000000000000000, 110.0000000000000000, 3.250000000000000444 ) ) ;
#3905 = SURFACE_SIDE_STYLE ('',( #3087 ) ) ;
#3906 = DIRECTION ( 'NONE',  ( -0.000000000000000000, 0.000000000000000000, 1.000000000000000000 ) ) ;
#3907 = ORIENTED_EDGE ( 'NONE', *, *, #11654, .F. ) ;
#3908 = CIRCLE ( 'NONE', #2115, 105.0000000000000426 ) ;
#3909 = ORIENTED_EDGE ( 'NONE', *, *, #2745, .T. ) ;
#3910 = AXIS2_PLACEMENT_3D ( 'NONE', #3558, #5558, #9397 ) ;
#3911 = CARTESIAN_POINT ( 'NONE',  ( 69.55864520994430222, 41.33566892181104890, -28.04631938806055658 ) ) ;
#3912 = VECTOR ( 'NONE', #8132, 1000.000000000000000 ) ;
#3913 = LINE ( 'NONE', #7470, #11466 ) ;
#3914 = CARTESIAN_POINT ( 'NONE',  ( -25.00000000000000000, 445.0000000000000568, -59.99999999999999289 ) ) ;
#3915 = FACE_OUTER_BOUND ( 'NONE', #2048, .T. ) ;
#3916 = DIRECTION ( 'NONE',  ( 0.000000000000000000, 1.000000000000000000, 0.000000000000000000 ) ) ;
#3917 = CARTESIAN_POINT ( 'NONE',  ( 70.44624282194224918, 13.32395845803458734, -25.73656789697610137 ) ) ;
#3918 = ORIENTED_EDGE ( 'NONE', *, *, #8323, .T. ) ;
#3919 = CARTESIAN_POINT ( 'NONE',  ( 0.000000000000000000, 275.0000000000000000, 0.000000000000000000 ) ) ;
#3920 = ADVANCED_FACE ( 'NONE', ( #2314, #6990 ), #4125, .T. ) ;
#3921 = CARTESIAN_POINT ( 'NONE',  ( 75.98513253586142469, 275.0000000000000000, 72.46557550663338532 ) ) ;
#3922 = VERTEX_POINT ( 'NONE', #1444 ) ;
#3923 = DIRECTION ( 'NONE',  ( 0.000000000000000000, 1.000000000000000000, 0.000000000000000000 ) ) ;
#3924 = VECTOR ( 'NONE', #10915, 1000.000000000000000 ) ;
#3925 = EDGE_CURVE ( 'NONE', #11877, #6026, #565, .T. ) ;
#3926 = VERTEX_POINT ( 'NONE', #8158 ) ;
#3927 = LINE ( 'NONE', #1929, #8108 ) ;
#3928 = CARTESIAN_POINT ( 'NONE',  ( 75.19960992036259029, 43.43221758413923794, 23.64972750892604481 ) ) ;
#3929 = VERTEX_POINT ( 'NONE', #5249 ) ;
#3930 = LINE ( 'NONE', #8775, #11854 ) ;
#3931 = DIRECTION ( 'NONE',  ( -0.4999999999999985567, -0.8660254037844394848, 0.000000000000000000 ) ) ;
#3932 = VERTEX_POINT ( 'NONE', #11734 ) ;
#3933 = DIRECTION ( 'NONE',  ( 0.000000000000000000, 1.000000000000000000, 0.000000000000000000 ) ) ;
#3934 = LINE ( 'NONE', #5685, #11191 ) ;
#3935 = LINE ( 'NONE', #9776, #7197 ) ;
#3936 = ORIENTED_EDGE ( 'NONE', *, *, #1598, .F. ) ;
#3937 = CARTESIAN_POINT ( 'NONE',  ( 2.708734124999999882, 113.2499999986344079, -1.121994411437820638 ) ) ;
#3938 = CARTESIAN_POINT ( 'NONE',  ( -5.970153145843347347E-16, 111.6249999972688158, -3.250000000000000444 ) ) ;
#3939 = ORIENTED_EDGE ( 'NONE', *, *, #3603, .T. ) ;
#3940 = CARTESIAN_POINT ( 'NONE',  ( 0.000000000000000000, 265.0000000000000000, 0.000000000000000000 ) ) ;
#3941 = DIRECTION ( 'NONE',  ( 0.000000000000000000, 1.000000000000000000, 0.000000000000000000 ) ) ;
#3942 = ORIENTED_EDGE ( 'NONE', *, *, #5719, .T. ) ;
#3943 = DIRECTION ( 'NONE',  ( 0.000000000000000000, -1.000000000000000000, 1.287488025362403787E-15 ) ) ;
#3944 = LINE ( 'NONE', #66, #11273 ) ;
#3945 = CIRCLE ( 'NONE', #4945, 9.999999999999998224 ) ;
#3946 = ORIENTED_EDGE ( 'NONE', *, *, #3184, .F. ) ;
#3947 = EDGE_CURVE ( 'NONE', #7739, #44, #3191, .T. ) ;
#3948 = CARTESIAN_POINT ( 'NONE',  ( -3.250000000000000444, 110.5000000000000000, 3.980102097228898231E-16 ) ) ;
#3949 = FACE_OUTER_BOUND ( 'NONE', #7911, .T. ) ;
#3950 = DIRECTION ( 'NONE',  ( -0.000000000000000000, -1.000000000000000000, -0.000000000000000000 ) ) ;
#3951 = DIRECTION ( 'NONE',  ( -0.4999999999999942268, 0.8660254037844419273, 0.000000000000000000 ) ) ;
#3952 = DIRECTION ( 'NONE',  ( 0.000000000000000000, 0.000000000000000000, 1.000000000000000000 ) ) ;
#3953 = ADVANCED_FACE ( 'NONE', ( #4305 ), #10789, .T. ) ;
#3954 = CARTESIAN_POINT ( 'NONE',  ( -1.915364268218908927, 112.9374999986344079, 1.915364268218909150 ) ) ;
#3955 = VERTEX_POINT ( 'NONE', #8098 ) ;
#3956 =( NAMED_UNIT ( * ) SI_UNIT ( $, .STERADIAN. ) SOLID_ANGLE_UNIT ( ) );
#3957 = ORIENTED_EDGE ( 'NONE', *, *, #4978, .F. ) ;
#3958 = DIRECTION ( 'NONE',  ( 0.000000000000000000, -0.000000000000000000, 1.000000000000000000 ) ) ;
#3959 = CARTESIAN_POINT ( 'NONE',  ( 25.00000000000000355, 450.0000000000000568, -105.0000000000000000 ) ) ;
#3960 = ORIENTED_EDGE ( 'NONE', *, *, #8475, .T. ) ;
#3961 = DIRECTION ( 'NONE',  ( 0.000000000000000000, -0.000000000000000000, 1.000000000000000000 ) ) ;
#3962 = FACE_OUTER_BOUND ( 'NONE', #12167, .T. ) ;
#3963 = CARTESIAN_POINT ( 'NONE',  ( -32.78711330112231792, 75.47285661897714704, 7.305343964218459440 ) ) ;
#3964 = CARTESIAN_POINT ( 'NONE',  ( 1.121994411437819528, 111.1249999986343937, -2.708734124999999882 ) ) ;
#3965 = EDGE_CURVE ( 'NONE', #3926, #11761, #8908, .T. ) ;
#3966 = ADVANCED_FACE ( 'NONE', ( #3498 ), #4613, .T. ) ;
#3967 = AXIS2_PLACEMENT_3D ( 'NONE', #10687, #5089, #2150 ) ;
#3968 = CARTESIAN_POINT ( 'NONE',  ( 74.58430552651930157, 42.25186411422790655, -24.46729545492062385 ) ) ;
#3969 = ADVANCED_FACE ( 'NONE', ( #3620 ), #1809, .T. ) ;
#3970 = CARTESIAN_POINT ( 'NONE',  ( 28.48065962374913695, 85.97961707684491728, 10.89289897176416666 ) ) ;
#3971 = FACE_OUTER_BOUND ( 'NONE', #5156, .T. ) ;
#3972 = ORIENTED_EDGE ( 'NONE', *, *, #2430, .F. ) ;
#3973 = DIRECTION ( 'NONE',  ( 0.000000000000000000, 1.000000000000000000, 0.000000000000000000 ) ) ;
#3974 = CARTESIAN_POINT ( 'NONE',  ( 71.26470115309105324, 16.39090745027094798, -23.55923316143329416 ) ) ;
#3975 = ORIENTED_EDGE ( 'NONE', *, *, #4758, .T. ) ;
#3976 = DIRECTION ( 'NONE',  ( 0.000000000000000000, -0.000000000000000000, 1.000000000000000000 ) ) ;
#3977 = CARTESIAN_POINT ( 'NONE',  ( -1.121994411437818862, 110.6249999986343937, 2.708734125000000326 ) ) ;
#3978 = VECTOR ( 'NONE', #6479, 1000.000000000000000 ) ;
#3979 = EDGE_LOOP ( 'NONE', ( #4172, #2289, #11702, #5545, #11579, #5316, #4614, #10830 ) ) ;
#3980 = CARTESIAN_POINT ( 'NONE',  ( -1.346194077712573822, 113.1874999972688016, 3.249999999999985789 ) ) ;
#3981 = EDGE_CURVE ( 'NONE', #10107, #6100, #7093, .T. ) ;
#3982 = ORIENTED_EDGE ( 'NONE', *, *, #4713, .F. ) ;
#3983 = ADVANCED_FACE ( 'NONE', ( #4672 ), #2502, .F. ) ;
#3984 = DIRECTION ( 'NONE',  ( -1.000000000000000000, -0.000000000000000000, -0.000000000000000000 ) ) ;
#3985 = AXIS2_PLACEMENT_3D ( 'NONE', #4502, #3253, #11930 ) ;
#3986 = LINE ( 'NONE', #6667, #250 ) ;
#3987 = EDGE_LOOP ( 'NONE', ( #10843, #4710, #9224, #4257, #7764 ) ) ;
#3988 = CARTESIAN_POINT ( 'NONE',  ( 25.00000000000000355, 450.0000000000000568, -105.0000000000000000 ) ) ;
#3989 = CARTESIAN_POINT ( 'NONE',  ( 27.96269517408201821, 86.23182228119654269, 11.42938571145646875 ) ) ;
#3990 = EDGE_LOOP ( 'NONE', ( #10978, #1858, #1559, #8988 ) ) ;
#3991 = ADVANCED_FACE ( 'NONE', ( #10216 ), #7038, .T. ) ;
#3992 = APPLICATION_PROTOCOL_DEFINITION ( 'draft international standard', 'automotive_design', 1998, #3181 ) ;
#3993 = CARTESIAN_POINT ( 'NONE',  ( 117.9289321881355193, 40.00000000000009237, -25.00000000000000000 ) ) ;
#3994 = DIRECTION ( 'NONE',  ( 0.000000000000000000, 0.000000000000000000, 1.000000000000000000 ) ) ;
#3995 = ORIENTED_EDGE ( 'NONE', *, *, #9433, .F. ) ;
#3996 = CARTESIAN_POINT ( 'NONE',  ( 1.121994411437818862, 112.4999999986344079, 2.708734125000000326 ) ) ;
#3997 = CARTESIAN_POINT ( 'NONE',  ( 1.990051048614449116E-16, 112.1249999972688158, 3.250000000000000444 ) ) ;
#3998 = CIRCLE ( 'NONE', #5596, 2.099999999999998312 ) ;
#3999 = ORIENTED_EDGE ( 'NONE', *, *, #4145, .T. ) ;
#4000 = DIRECTION ( 'NONE',  ( -1.224646799147354193E-16, 0.000000000000000000, -1.000000000000000000 ) ) ;
#4001 = DIRECTION ( 'NONE',  ( -0.000000000000000000, -1.000000000000000000, -0.000000000000000000 ) ) ;
#4002 = ORIENTED_EDGE ( 'NONE', *, *, #3213, .F. ) ;
#4003 = CARTESIAN_POINT ( 'NONE',  ( -13.00000000000000178, 170.0000000000000000, -7.483314773547880883 ) ) ;
#4004 = AXIS2_PLACEMENT_3D ( 'NONE', #10613, #10676, #5887 ) ;
#4005 = VECTOR ( 'NONE', #2690, 1000.000000000000000 ) ;
#4006 = ORIENTED_EDGE ( 'NONE', *, *, #6267, .T. ) ;
#4007 = CARTESIAN_POINT ( 'NONE',  ( -1.346194077712555837, 110.6875000000000000, -3.250000000000004885 ) ) ;
#4008 = PLANE ( 'NONE',  #1732 ) ;
#4009 = DIRECTION ( 'NONE',  ( 0.000000000000000000, 1.000000000000000000, 0.000000000000000000 ) ) ;
#4010 = CARTESIAN_POINT ( 'NONE',  ( 117.9289321881355193, 50.00000000000008527, -25.00000000000000000 ) ) ;
#4011 = LINE ( 'NONE', #3137, #7949 ) ;
#4012 = CIRCLE ( 'NONE', #4403, 5.000000000000000888 ) ;
#4013 = CARTESIAN_POINT ( 'NONE',  ( 2.708734124999999437, 113.4999999986344079, -1.121994411437820416 ) ) ;
#4014 = VECTOR ( 'NONE', #492, 1000.000000000000000 ) ;
#4015 = ORIENTED_EDGE ( 'NONE', *, *, #1431, .T. ) ;
#4016 = EDGE_CURVE ( 'NONE', #4117, #8618, #1720, .T. ) ;
#4017 = EDGE_LOOP ( 'NONE', ( #11299, #4724, #4108, #5693 ) ) ;
#4018 = DIRECTION ( 'NONE',  ( -1.000000000000000000, -0.000000000000000000, -0.000000000000000000 ) ) ;
#4019 = CARTESIAN_POINT ( 'NONE',  ( 10.45882351999534521, 39.49462622639263287, 74.26988840762503230 ) ) ;
#4020 = VERTEX_POINT ( 'NONE', #8466 ) ;
#4021 = VECTOR ( 'NONE', #7145, 1000.000000000000000 ) ;
#4022 = ADVANCED_FACE ( 'NONE', ( #4427 ), #6548, .F. ) ;
#4023 = DIRECTION ( 'NONE',  ( -0.4999999999999933387, 0.8660254037844424824, 0.000000000000000000 ) ) ;
#4024 = PLANE ( 'NONE',  #2368 ) ;
#4025 = ADVANCED_FACE ( 'NONE', ( #4550 ), #1567, .T. ) ;
#4026 = AXIS2_PLACEMENT_3D ( 'NONE', #7490, #3683, #11301 ) ;
#4027 = CARTESIAN_POINT ( 'NONE',  ( -30.49437064397536901, 76.52118294276679933, 5.489589508502957571 ) ) ;
#4028 = DIRECTION ( 'NONE',  ( 0.000000000000000000, 1.000000000000000000, 0.000000000000000000 ) ) ;
#4029 = EDGE_LOOP ( 'NONE', ( #8804, #4229, #9177, #1653, #10623, #205, #5758, #3565 ) ) ;
#4030 = AXIS2_PLACEMENT_3D ( 'NONE', #3395, #5679, #1584 ) ;
#4031 = DIRECTION ( 'NONE',  ( -0.000000000000000000, -1.000000000000000000, -0.000000000000000000 ) ) ;
#4032 = EDGE_CURVE ( 'NONE', #5307, #10772, #11206, .T. ) ;
#4033 = FACE_OUTER_BOUND ( 'NONE', #2610, .T. ) ;
#4034 = CARTESIAN_POINT ( 'NONE',  ( -25.00000000000000000, 445.0000000000000568, -29.99999999999999289 ) ) ;
#4035 = ORIENTED_EDGE ( 'NONE', *, *, #9787, .F. ) ;
#4036 = B_SPLINE_CURVE_WITH_KNOTS ( 'NONE', 3,
 ( #2606, #12214, #3545, #2852 ),
 .UNSPECIFIED., .F., .F.,
 ( 4, 4 ),
 ( 0.0002502309401078630247, 0.0005002309401076750293 ),
 .UNSPECIFIED. ) ;
#4037 = LINE ( 'NONE', #11897, #1702 ) ;
#4038 = CARTESIAN_POINT ( 'NONE',  ( 71.69683552452198683, 10.62043640550095702, -22.01474836615561514 ) ) ;
#4039 = ORIENTED_EDGE ( 'NONE', *, *, #6697, .T. ) ;
#4040 = DIRECTION ( 'NONE',  ( -0.000000000000000000, 1.000000000000000000, -0.000000000000000000 ) ) ;
#4041 = DIRECTION ( 'NONE',  ( 0.000000000000000000, 0.000000000000000000, -1.000000000000000000 ) ) ;
#4042 = AXIS2_PLACEMENT_3D ( 'NONE', #9843, #8032, #1319 ) ;
#4043 = ORIENTED_EDGE ( 'NONE', *, *, #1673, .F. ) ;
#4044 = CARTESIAN_POINT ( 'NONE',  ( -2.298097038856279806, 113.4999999972688158, -2.298097038856279362 ) ) ;
#4045 = ADVANCED_FACE ( 'NONE', ( #11165 ), #1629, .F. ) ;
#4046 = EDGE_CURVE ( 'NONE', #5931, #8932, #9265, .T. ) ;
#4047 = VERTEX_POINT ( 'NONE', #10336 ) ;
#4048 = AXIS2_PLACEMENT_3D ( 'NONE', #7472, #9261, #3480 ) ;
#4049 = CARTESIAN_POINT ( 'NONE',  ( 21.00000000000000355, 0.000000000000000000, 0.000000000000000000 ) ) ;
#4050 = DIRECTION ( 'NONE',  ( 1.000000000000000000, 0.000000000000000000, 0.000000000000000000 ) ) ;
#4051 = ORIENTED_EDGE ( 'NONE', *, *, #3073, .F. ) ;
#4052 = CARTESIAN_POINT ( 'NONE',  ( 25.00000000000000000, 345.0000000000000568, -29.99999999999998934 ) ) ;
#4053 = DIRECTION ( 'NONE',  ( 0.000000000000000000, 1.000000000000000000, 0.000000000000000000 ) ) ;
#4054 = ORIENTED_EDGE ( 'NONE', *, *, #584, .F. ) ;
#4055 = LINE ( 'NONE', #1997, #10823 ) ;
#4056 = DIRECTION ( 'NONE',  ( 0.9595199576812789566, 0.000000000000000000, 0.2816406412635021894 ) ) ;
#4057 = ORIENTED_EDGE ( 'NONE', *, *, #9903, .T. ) ;
#4058 = CARTESIAN_POINT ( 'NONE',  ( 1.915364268218908927, 111.1874999986344079, -1.915364268218909816 ) ) ;
#4059 = VECTOR ( 'NONE', #4091, 1000.000000000000000 ) ;
#4060 = FACE_OUTER_BOUND ( 'NONE', #7414, .T. ) ;
#4061 = ADVANCED_FACE ( 'NONE', ( #12044 ), #692, .T. ) ;
#4062 = VERTEX_POINT ( 'NONE', #5801 ) ;
#4063 = CARTESIAN_POINT ( 'NONE',  ( 7.344472908538985045, 35.21650635094629678, 79.50000000000000000 ) ) ;
#4064 = CARTESIAN_POINT ( 'NONE',  ( 170.0000000000011369, 35.00000000000004974, 20.00000000000000000 ) ) ;
#4065 = VERTEX_POINT ( 'NONE', #9462 ) ;
#4066 = CARTESIAN_POINT ( 'NONE',  ( 25.00000000000000000, 450.0000000000000568, -59.99999999999999289 ) ) ;
#4067 = CARTESIAN_POINT ( 'NONE',  ( 0.000000000000000000, 165.0000000000000000, 0.000000000000000000 ) ) ;
#4068 = ORIENTED_EDGE ( 'NONE', *, *, #8855, .F. ) ;
#4069 = AXIS2_PLACEMENT_3D ( 'NONE', #3585, #5277, #5400 ) ;
#4070 = DIRECTION ( 'NONE',  ( 0.000000000000000000, 1.000000000000000000, 0.000000000000000000 ) ) ;
#4071 = AXIS2_PLACEMENT_3D ( 'NONE', #6165, #6047, #9015 ) ;
#4072 = CARTESIAN_POINT ( 'NONE',  ( 10.19254911989241386, 23.71650635094626836, 79.50000000000000000 ) ) ;
#4073 = DIRECTION ( 'NONE',  ( 0.000000000000000000, 0.000000000000000000, 1.000000000000000000 ) ) ;
#4074 = EDGE_LOOP ( 'NONE', ( #11181, #2184, #4452, #11858, #1078 ) ) ;
#4075 = FACE_OUTER_BOUND ( 'NONE', #1348, .T. ) ;
#4076 = ADVANCED_FACE ( 'NONE', ( #3801 ), #1894, .F. ) ;
#4077 = CARTESIAN_POINT ( 'NONE',  ( -1.121994411437820194, 113.2499999986344079, -2.708734124999999437 ) ) ;
#4078 = VERTEX_POINT ( 'NONE', #2802 ) ;
#4079 = ORIENTED_EDGE ( 'NONE', *, *, #8272, .F. ) ;
#4080 = DIRECTION ( 'NONE',  ( -1.000000000000000000, -0.000000000000000000, -0.000000000000000000 ) ) ;
#4081 = CARTESIAN_POINT ( 'NONE',  ( 11.99804506437387985, 37.16050278248236793, 74.03439849576338361 ) ) ;
#4082 = VERTEX_POINT ( 'NONE', #9586 ) ;
#4083 = DIRECTION ( 'NONE',  ( 0.000000000000000000, 0.000000000000000000, 1.000000000000000000 ) ) ;
#4084 = FACE_BOUND ( 'NONE', #1405, .T. ) ;
#4085 = CARTESIAN_POINT ( 'NONE',  ( 74.16198487095665826, 40.00000000000009237, -30.00000000000000355 ) ) ;
#4086 = VECTOR ( 'NONE', #10264, 1000.000000000000000 ) ;
#4087 = VECTOR ( 'NONE', #12233, 1000.000000000000000 ) ;
#4088 = EDGE_CURVE ( 'NONE', #3422, #65, #4469, .T. ) ;
#4089 = EDGE_CURVE ( 'NONE', #12119, #10896, #3930, .T. ) ;
#4090 = DIRECTION ( 'NONE',  ( 0.000000000000000000, 0.000000000000000000, -1.000000000000000000 ) ) ;
#4091 = DIRECTION ( 'NONE',  ( -0.000000000000000000, 1.000000000000000000, -0.000000000000000000 ) ) ;
#4092 = DIRECTION ( 'NONE',  ( -0.000000000000000000, 1.000000000000000000, -0.000000000000000000 ) ) ;
#4093 = CLOSED_SHELL ( 'NONE', ( #8608, #5884, #8379, #6886, #5244, #11748, #9530, #3099, #7111, #5011, #10173, #9366, #12157, #12080, #4025, #1369, #10673, #1774, #8962, #10457, #7797, #5037, #5063, #3983, #3434, #5067, #7390 ) ) ;
#4094 = VECTOR ( 'NONE', #3426, 1000.000000000000114 ) ;
#4095 = PLANE ( 'NONE',  #12067 ) ;
#4096 = CARTESIAN_POINT ( 'NONE',  ( 72.45821416003295212, 14.86625829596107984, -19.37058730516337235 ) ) ;
#4097 = DIRECTION ( 'NONE',  ( 0.000000000000000000, 0.000000000000000000, 1.000000000000000000 ) ) ;
#4098 = PRODUCT_DEFINITION_SHAPE ( 'NONE', 'NONE',  #12359 ) ;
#4099 = CARTESIAN_POINT ( 'NONE',  ( 2.708734124999999882, 111.2499999986344079, -1.121994411437820638 ) ) ;
#4100 = AXIS2_PLACEMENT_3D ( 'NONE', #1884, #3574, #11250 ) ;
#4101 = ORIENTED_EDGE ( 'NONE', *, *, #11893, .T. ) ;
#4102 = CARTESIAN_POINT ( 'NONE',  ( 20.55500000000001748, 0.000000000000000000, 0.000000000000000000 ) ) ;
#4103 = EDGE_CURVE ( 'NONE', #11144, #8201, #11367, .T. ) ;
#4104 = EDGE_CURVE ( 'NONE', #2993, #2376, #1993, .T. ) ;
#4105 = AXIS2_PLACEMENT_3D ( 'NONE', #4864, #8651, #3931 ) ;
#4106 = ORIENTED_EDGE ( 'NONE', *, *, #10124, .F. ) ;
#4107 = DIRECTION ( 'NONE',  ( -0.000000000000000000, -0.000000000000000000, -1.000000000000000000 ) ) ;
#4108 = ORIENTED_EDGE ( 'NONE', *, *, #8493, .T. ) ;
#4109 = CARTESIAN_POINT ( 'NONE',  ( 135.0000000000011084, 67.07106781186550393, 20.00000000000000000 ) ) ;
#4110 = LINE ( 'NONE', #240, #4298 ) ;
#4111 = ORIENTED_EDGE ( 'NONE', *, *, #2239, .F. ) ;
#4112 = DIRECTION ( 'NONE',  ( 0.000000000000000000, 0.000000000000000000, -1.000000000000000000 ) ) ;
#4113 = AXIS2_PLACEMENT_3D ( 'NONE', #9930, #3148, #9050 ) ;
#4114 = LINE ( 'NONE', #8594, #10164 ) ;
#4115 = EDGE_CURVE ( 'NONE', #6843, #1004, #6870, .T. ) ;
#4116 =( BOUNDED_CURVE ( )  B_SPLINE_CURVE ( 3, ( #2297, #9769, #7899, #1364 ),
 .UNSPECIFIED., .F., .F. ) 
 B_SPLINE_CURVE_WITH_KNOTS ( ( 4, 4 ),
 ( 1.666086958916892291, 1.694832046014206117 ),
 .UNSPECIFIED. ) 
 CURVE ( )  GEOMETRIC_REPRESENTATION_ITEM ( )  RATIONAL_B_SPLINE_CURVE ( ( 1.000000000000000000, 0.9999311445159493328, 0.9999311445159493328, 1.000000000000000000 ) ) 
 REPRESENTATION_ITEM ( '' )  );
#4117 = VERTEX_POINT ( 'NONE', #1003 ) ;
#4118 = CARTESIAN_POINT ( 'NONE',  ( -1.915364268218909816, 112.9374999986344079, -1.915364268218909150 ) ) ;
#4119 = CARTESIAN_POINT ( 'NONE',  ( -3.250000000000000444, 114.3749999972688158, 3.980102097228898231E-16 ) ) ;
#4120 = ORIENTED_EDGE ( 'NONE', *, *, #3352, .T. ) ;
#4121 = CARTESIAN_POINT ( 'NONE',  ( 29.71888078761409346, 87.31388704012290702, 9.203922339174773981 ) ) ;
#4122 = DIRECTION ( 'NONE',  ( 0.000000000000000000, 0.000000000000000000, 1.000000000000000000 ) ) ;
#4123 = ORIENTED_EDGE ( 'NONE', *, *, #7393, .T. ) ;
#4124 = DIRECTION ( 'NONE',  ( -0.000000000000000000, -1.000000000000000000, -0.000000000000000000 ) ) ;
#4125 = PLANE ( 'NONE',  #9058 ) ;
#4126 = ORIENTED_EDGE ( 'NONE', *, *, #3169, .T. ) ;
#4127 = CARTESIAN_POINT ( 'NONE',  ( -31.74999999999995737, 0.000000000000000000, 0.000000000000000000 ) ) ;
#4128 = CARTESIAN_POINT ( 'NONE',  ( 76.59657895567488595, 44.76487798575835342, -21.54700147973310820 ) ) ;
#4129 = DIRECTION ( 'NONE',  ( 0.000000000000000000, 1.000000000000000000, 0.000000000000000000 ) ) ;
#4130 = ORIENTED_EDGE ( 'NONE', *, *, #2970, .T. ) ;
#4131 = CARTESIAN_POINT ( 'NONE',  ( -82.90657655639077461, 275.0000000000000000, 79.06642500897154946 ) ) ;
#4132 = CARTESIAN_POINT ( 'NONE',  ( 74.98307306353127899, 16.90879164695958892, 23.94359236838928240 ) ) ;
#4133 = ORIENTED_EDGE ( 'NONE', *, *, #5258, .F. ) ;
#4134 = FACE_OUTER_BOUND ( 'NONE', #1861, .T. ) ;
#4135 = VERTEX_POINT ( 'NONE', #7725 ) ;
#4136 = EDGE_CURVE ( 'NONE', #3575, #7739, #10652, .T. ) ;
#4137 = CARTESIAN_POINT ( 'NONE',  ( 5.524523187418616033, 41.13124826485281460, 80.00000000000000000 ) ) ;
#4138 = EDGE_CURVE ( 'NONE', #7105, #11220, #11538, .T. ) ;
#4139 = CARTESIAN_POINT ( 'NONE',  ( 69.55283199277504025, 41.34318640236479325, 28.06103394134322571 ) ) ;
#4140 = ORIENTED_EDGE ( 'NONE', *, *, #3877, .F. ) ;
#4141 = CARTESIAN_POINT ( 'NONE',  ( 5.237050087044693214, 18.70000308413499823, 80.00000000000000000 ) ) ;
#4142 = DIRECTION ( 'NONE',  ( -0.000000000000000000, -0.000000000000000000, 1.000000000000000000 ) ) ;
#4143 = CARTESIAN_POINT ( 'NONE',  ( 0.000000000000000000, 109.0000000000000000, 0.000000000000000000 ) ) ;
#4144 = CARTESIAN_POINT ( 'NONE',  ( 0.000000000000000000, 65.00000000000000000, 0.000000000000000000 ) ) ;
#4145 = EDGE_CURVE ( 'NONE', #945, #931, #330, .T. ) ;
#4146 = AXIS2_PLACEMENT_3D ( 'NONE', #7722, #11535, #6605 ) ;
#4147 =( GEOMETRIC_REPRESENTATION_CONTEXT ( 3 ) GLOBAL_UNCERTAINTY_ASSIGNED_CONTEXT ( ( #11394 ) ) GLOBAL_UNIT_ASSIGNED_CONTEXT ( ( #967, #3895, #6821 ) ) REPRESENTATION_CONTEXT ( 'NONE', 'WORKASPACE' ) );
#4148 = VERTEX_POINT ( 'NONE', #11479 ) ;
#4149 =( NAMED_UNIT ( * ) SI_UNIT ( $, .STERADIAN. ) SOLID_ANGLE_UNIT ( ) );
#4150 = ORIENTED_EDGE ( 'NONE', *, *, #9309, .T. ) ;
#4151 = FACE_OUTER_BOUND ( 'NONE', #667, .T. ) ;
#4152 = DIRECTION ( 'NONE',  ( -0.000000000000000000, 1.000000000000000000, -0.000000000000000000 ) ) ;
#4153 = DIRECTION ( 'NONE',  ( 0.000000000000000000, 0.000000000000000000, 1.000000000000000000 ) ) ;
#4154 = FACE_OUTER_BOUND ( 'NONE', #7451, .T. ) ;
#4155 = DIRECTION ( 'NONE',  ( 0.000000000000000000, 0.000000000000000000, 1.000000000000000000 ) ) ;
#4156 = CARTESIAN_POINT ( 'NONE',  ( -1.346194077712559389, 110.3125000000000142, 3.250000000000000444 ) ) ;
#4157 = ORIENTED_EDGE ( 'NONE', *, *, #5520, .T. ) ;
#4158 = DIRECTION ( 'NONE',  ( -0.000000000000000000, -1.000000000000000000, -0.000000000000000000 ) ) ;
#4159 = EDGE_CURVE ( 'NONE', #3527, #3436, #2931, .T. ) ;
#4160 = ORIENTED_EDGE ( 'NONE', *, *, #7644, .T. ) ;
#4161 = LINE ( 'NONE', #5114, #12221 ) ;
#4162 = VERTEX_POINT ( 'NONE', #7785 ) ;
#4163 = CARTESIAN_POINT ( 'NONE',  ( -5.970153145843347347E-16, 112.6249999972688158, -3.250000000000000444 ) ) ;
#4164 = DIRECTION ( 'NONE',  ( 0.000000000000000000, 1.000000000000000000, 0.000000000000000000 ) ) ;
#4165 = ORIENTED_EDGE ( 'NONE', *, *, #2791, .F. ) ;
#4166 = EDGE_CURVE ( 'NONE', #5753, #9534, #10242, .T. ) ;
#4167 = AXIS2_PLACEMENT_3D ( 'NONE', #8149, #11971, #8898 ) ;
#4168 = CIRCLE ( 'NONE', #11343, 70.00000000000001421 ) ;
#4169 = CARTESIAN_POINT ( 'NONE',  ( 0.000000000000000000, 65.00000000000000000, 90.00000000000002842 ) ) ;
#4170 = PRESENTATION_LAYER_ASSIGNMENT (  '', '', ( #1985 ) ) ;
#4171 = CARTESIAN_POINT ( 'NONE',  ( -29.71888078761410767, 87.31388704012290702, -9.203922339174775757 ) ) ;
#4172 = ORIENTED_EDGE ( 'NONE', *, *, #4544, .F. ) ;
#4173 = DIRECTION ( 'NONE',  ( -0.000000000000000000, -1.000000000000000000, -0.000000000000000000 ) ) ;
#4174 = VECTOR ( 'NONE', #7419, 1000.000000000000000 ) ;
#4175 = ORIENTED_EDGE ( 'NONE', *, *, #4419, .F. ) ;
#4176 = EDGE_CURVE ( 'NONE', #10404, #9390, #7843, .T. ) ;
#4177 = DIRECTION ( 'NONE',  ( 0.000000000000000000, 1.000000000000000000, 0.000000000000000000 ) ) ;
#4178 = CARTESIAN_POINT ( 'NONE',  ( 3.061616997868383043E-15, 67.00000000000000000, -25.00000000000000000 ) ) ;
#4179 = EDGE_CURVE ( 'NONE', #9892, #5904, #87, .T. ) ;
#4180 = ORIENTED_EDGE ( 'NONE', *, *, #4410, .F. ) ;
#4181 = VECTOR ( 'NONE', #6753, 1000.000000000000000 ) ;
#4182 = CARTESIAN_POINT ( 'NONE',  ( 117.9289321881355193, 50.00000000000008527, 25.00000000000000000 ) ) ;
#4183 = CARTESIAN_POINT ( 'NONE',  ( 140.0000000000011369, 230.0000000000000853, 25.00000000000000000 ) ) ;
#4184 = ORIENTED_EDGE ( 'NONE', *, *, #854, .T. ) ;
#4185 = DIRECTION ( 'NONE',  ( 0.000000000000000000, 1.000000000000000000, 0.000000000000000000 ) ) ;
#4186 = CYLINDRICAL_SURFACE ( 'NONE', #6111, 28.00000000000000355 ) ;
#4187 = CARTESIAN_POINT ( 'NONE',  ( 0.000000000000000000, 92.00000000000000000, 0.000000000000000000 ) ) ;
#4188 = VECTOR ( 'NONE', #9316, 1000.000000000000114 ) ;
#4189 = ORIENTED_EDGE ( 'NONE', *, *, #5828, .T. ) ;
#4190 = CARTESIAN_POINT ( 'NONE',  ( 0.000000000000000000, 110.0000000000000000, 0.000000000000000000 ) ) ;
#4191 = AXIS2_PLACEMENT_3D ( 'NONE', #3772, #5777, #5715 ) ;
#4192 = CARTESIAN_POINT ( 'NONE',  ( 74.16198487097054226, 19.83292322748416581, 25.00000000000000000 ) ) ;
#4193 = EDGE_CURVE ( 'NONE', #9087, #3178, #4881, .T. ) ;
#4194 = EDGE_LOOP ( 'NONE', ( #6253, #7438 ) ) ;
#4195 = ADVANCED_FACE ( 'NONE', ( #2419 ), #10775, .F. ) ;
#4196 = CARTESIAN_POINT ( 'NONE',  ( 0.000000000000000000, 65.00000000000000000, 0.000000000000000000 ) ) ;
#4197 = EDGE_CURVE ( 'NONE', #6619, #3427, #4675, .T. ) ;
#4198 = CARTESIAN_POINT ( 'NONE',  ( 75.38685631124155861, 43.68135433386650135, -23.38733102174701983 ) ) ;
#4199 = ORIENTED_EDGE ( 'NONE', *, *, #6254, .F. ) ;
#4200 = DIRECTION ( 'NONE',  ( -1.000000000000000000, 3.469446951953611033E-15, 0.000000000000000000 ) ) ;
#4201 = CARTESIAN_POINT ( 'NONE',  ( 69.52686081652184669, 40.00000000000009237, 28.12500000000000000 ) ) ;
#4202 = ORIENTED_EDGE ( 'NONE', *, *, #10975, .T. ) ;
#4203 = LINE ( 'NONE', #2149, #6222 ) ;
#4204 = CARTESIAN_POINT ( 'NONE',  ( 0.000000000000000000, 75.00000000000001421, 0.000000000000000000 ) ) ;
#4205 = DIRECTION ( 'NONE',  ( 6.938893903907222067E-15, 1.000000000000000000, 0.000000000000000000 ) ) ;
#4206 = CARTESIAN_POINT ( 'NONE',  ( -2.708734125000000326, 110.8124999986344079, 3.317242575922457132E-16 ) ) ;
#4207 = AXIS2_PLACEMENT_3D ( 'NONE', #1918, #2105, #9570 ) ;
#4208 = VECTOR ( 'NONE', #10220, 1000.000000000000000 ) ;
#4209 = ORIENTED_EDGE ( 'NONE', *, *, #3515, .T. ) ;
#4210 = ORIENTED_EDGE ( 'NONE', *, *, #2844, .T. ) ;
#4211 = SURFACE_STYLE_FILL_AREA ( #7706 ) ;
#4212 = VERTEX_POINT ( 'NONE', #6226 ) ;
#4213 = EDGE_CURVE ( 'NONE', #6665, #7233, #5280, .T. ) ;
#4214 = SURFACE_STYLE_USAGE ( .BOTH. , #8995 ) ;
#4215 = AXIS2_PLACEMENT_3D ( 'NONE', #10092, #4555, #9340 ) ;
#4216 = CARTESIAN_POINT ( 'NONE',  ( 117.9289321881355193, 50.00000000000008527, 20.00000000000000000 ) ) ;
#4217 = CARTESIAN_POINT ( 'NONE',  ( 2.500000000000000000, -2.357898499370432166, 3.035766082959412415E-15 ) ) ;
#4218 = CARTESIAN_POINT ( 'NONE',  ( 0.000000000000000000, 265.0000000000000000, 0.000000000000000000 ) ) ;
#4219 = SHAPE_DEFINITION_REPRESENTATION ( #7872, #12244 ) ;
#4220 = CARTESIAN_POINT ( 'NONE',  ( 3.367778697655220913E-15, 92.00000000000000000, -24.99999999999999645 ) ) ;
#4221 = CARTESIAN_POINT ( 'NONE',  ( 2.708734124999999882, 112.2499999986344079, -1.121994411437820638 ) ) ;
#4222 = VERTEX_POINT ( 'NONE', #6974 ) ;
#4223 = CARTESIAN_POINT ( 'NONE',  ( 0.000000000000000000, 110.0000000000000000, 0.000000000000000000 ) ) ;
#4224 = EDGE_CURVE ( 'NONE', #8106, #8030, #8444, .T. ) ;
#4225 = ORIENTED_EDGE ( 'NONE', *, *, #7597, .T. ) ;
#4226 = DIRECTION ( 'NONE',  ( 0.000000000000000000, 0.000000000000000000, 1.000000000000000000 ) ) ;
#4227 = ORIENTED_EDGE ( 'NONE', *, *, #10004, .F. ) ;
#4228 = DIRECTION ( 'NONE',  ( -0.000000000000000000, 1.000000000000000000, -0.000000000000000000 ) ) ;
#4229 = ORIENTED_EDGE ( 'NONE', *, *, #6676, .T. ) ;
#4230 = CIRCLE ( 'NONE', #1838, 9.999999999999994671 ) ;
#4231 = LINE ( 'NONE', #10778, #2075 ) ;
#4232 = LINE ( 'NONE', #2238, #4014 ) ;
#4233 = ORIENTED_EDGE ( 'NONE', *, *, #11292, .T. ) ;
#4234 = CIRCLE ( 'NONE', #11217, 5.000000000000000000 ) ;
#4235 = ADVANCED_FACE ( 'NONE', ( #7958 ), #3089, .T. ) ;
#4236 = ADVANCED_FACE ( 'NONE', ( #2232 ), #9893, .T. ) ;
#4237 = ORIENTED_EDGE ( 'NONE', *, *, #11667, .F. ) ;
#4238 = CARTESIAN_POINT ( 'NONE',  ( 0.000000000000000000, 170.0000000000000000, 0.000000000000000000 ) ) ;
#4239 = CARTESIAN_POINT ( 'NONE',  ( 69.52686081652184669, 20.00000000000009237, 28.12499999999999645 ) ) ;
#4240 = EDGE_LOOP ( 'NONE', ( #4506, #7187, #4921, #4359 ) ) ;
#4241 = FACE_OUTER_BOUND ( 'NONE', #10331, .T. ) ;
#4242 = DIRECTION ( 'NONE',  ( -0.2358520287683112115, 0.000000000000000000, -0.9717889794219070065 ) ) ;
#4243 = ORIENTED_EDGE ( 'NONE', *, *, #9744, .T. ) ;
#4244 = FACE_OUTER_BOUND ( 'NONE', #4272, .T. ) ;
#4245 = LINE ( 'NONE', #10792, #2322 ) ;
#4246 = DIRECTION ( 'NONE',  ( -1.000000000000000000, 3.469446951953611033E-15, 0.000000000000000000 ) ) ;
#4247 = VECTOR ( 'NONE', #2976, 1000.000000000000114 ) ;
#4248 = ORIENTED_EDGE ( 'NONE', *, *, #39, .F. ) ;
#4249 = CARTESIAN_POINT ( 'NONE',  ( 28.12254474901590484, 87.93978760833334718, 10.28801392380147206 ) ) ;
#4250 = CARTESIAN_POINT ( 'NONE',  ( 70.92179708824001239, 12.01015086585302960, 24.39594572817764373 ) ) ;
#4251 = ADVANCED_FACE ( 'NONE', ( #8021, #10897 ), #5984, .T. ) ;
#4252 = ORIENTED_EDGE ( 'NONE', *, *, #8293, .T. ) ;
#4253 = PLANE ( 'NONE',  #5673 ) ;
#4254 = DIRECTION ( 'NONE',  ( 0.000000000000000000, 0.000000000000000000, 1.000000000000000000 ) ) ;
#4255 = AXIS2_PLACEMENT_3D ( 'NONE', #9676, #4957, #3958 ) ;
#4256 = VECTOR ( 'NONE', #2807, 1000.000000000000000 ) ;
#4257 = ORIENTED_EDGE ( 'NONE', *, *, #10379, .T. ) ;
#4258 = EDGE_CURVE ( 'NONE', #10229, #945, #4116, .T. ) ;
#4259 = CARTESIAN_POINT ( 'NONE',  ( 3.250000000000000444, 111.0624999999999858, 1.346194077712559167 ) ) ;
#4260 = CARTESIAN_POINT ( 'NONE',  ( 70.23094937779826807, 45.91093084162184823, 26.31821466697815382 ) ) ;
#4261 = EDGE_LOOP ( 'NONE', ( #3907, #3081, #4794, #9086 ) ) ;
#4262 = LINE ( 'NONE', #458, #10394 ) ;
#4263 = DIRECTION ( 'NONE',  ( 0.000000000000000000, 0.000000000000000000, -1.000000000000000000 ) ) ;
#4264 = FACE_OUTER_BOUND ( 'NONE', #11353, .T. ) ;
#4265 = CYLINDRICAL_SURFACE ( 'NONE', #3402, 75.00000000000002842 ) ;
#4266 = EDGE_CURVE ( 'NONE', #6100, #10107, #1100, .T. ) ;
#4267 = EDGE_CURVE ( 'NONE', #11144, #3256, #4289, .T. ) ;
#4268 = AXIS2_PLACEMENT_3D ( 'NONE', #9352, #11369, #837 ) ;
#4269 = ORIENTED_EDGE ( 'NONE', *, *, #3887, .T. ) ;
#4270 = PRESENTATION_STYLE_ASSIGNMENT (( #1469 ) ) ;
#4271 = VECTOR ( 'NONE', #2045, 1000.000000000000114 ) ;
#4272 = EDGE_LOOP ( 'NONE', ( #10114, #7259, #2067, #3644 ) ) ;
#4273 = CARTESIAN_POINT ( 'NONE',  ( 117.9289321881355193, 50.00000000000008527, 20.00000000000000000 ) ) ;
#4274 = CARTESIAN_POINT ( 'NONE',  ( 2.500000000000000000, -1.178949249685218748, -2.041999999999998039 ) ) ;
#4275 = DIRECTION ( 'NONE',  ( -0.5000000000000036637, -0.8660254037844364872, 0.000000000000000000 ) ) ;
#4276 = CIRCLE ( 'NONE', #8046, 2.649999999999993694 ) ;
#4277 = CARTESIAN_POINT ( 'NONE',  ( -27.67899820261485999, 88.38261385519929547, -11.05501148229834030 ) ) ;
#4278 = VECTOR ( 'NONE', #9042, 1000.000000000000000 ) ;
#4279 = LINE ( 'NONE', #9694, #2292 ) ;
#4280 = PLANE ( 'NONE',  #6102 ) ;
#4281 = CARTESIAN_POINT ( 'NONE',  ( 11.02471948819644965, 21.24513208498732908, 74.18696493688197791 ) ) ;
#4282 = CARTESIAN_POINT ( 'NONE',  ( -89.80805993797480369, 275.0000000000000000, 81.82974571984181011 ) ) ;
#4283 = CARTESIAN_POINT ( 'NONE',  ( -1.121994411437820416, 111.9999999986343937, -2.708734124999999882 ) ) ;
#4284 = CARTESIAN_POINT ( 'NONE',  ( -25.00000000000000000, 445.0000000000000568, -59.99999999999999289 ) ) ;
#4285 = DIRECTION ( 'NONE',  ( 0.000000000000000000, 0.000000000000000000, 1.000000000000000000 ) ) ;
#4286 = ORIENTED_EDGE ( 'NONE', *, *, #3308, .T. ) ;
#4287 = DIRECTION ( 'NONE',  ( -0.5000000000000001110, -0.8660254037844387076, 0.000000000000000000 ) ) ;
#4288 = EDGE_LOOP ( 'NONE', ( #4983, #1979, #8497, #8960 ) ) ;
#4289 = LINE ( 'NONE', #8894, #9638 ) ;
#4290 = EDGE_CURVE ( 'NONE', #7703, #10799, #4276, .T. ) ;
#4291 = CARTESIAN_POINT ( 'NONE',  ( 120.0000000000009948, 45.00000000000008527, 25.00000000000000000 ) ) ;
#4292 = EDGE_LOOP ( 'NONE', ( #3803, #8683 ) ) ;
#4293 = DIRECTION ( 'NONE',  ( 0.000000000000000000, -1.000000000000000000, 0.000000000000000000 ) ) ;
#4294 = DIRECTION ( 'NONE',  ( 0.000000000000000000, 0.000000000000000000, 1.000000000000000000 ) ) ;
#4295 = ADVANCED_FACE ( 'NONE', ( #3363 ), #11258, .F. ) ;
#4296 = ORIENTED_EDGE ( 'NONE', *, *, #10472, .T. ) ;
#4297 = CARTESIAN_POINT ( 'NONE',  ( -3.250000000000000444, 113.5000000000000000, 3.980102097228898231E-16 ) ) ;
#4298 = VECTOR ( 'NONE', #2992, 1000.000000000000114 ) ;
#4299 = EDGE_LOOP ( 'NONE', ( #7130, #2764, #4727, #2173, #1393 ) ) ;
#4300 = DIRECTION ( 'NONE',  ( 1.000000000000000000, 0.000000000000000000, 0.000000000000000000 ) ) ;
#4301 = DIRECTION ( 'NONE',  ( 0.7071067811865447972, -0.7071067811865503483, 0.000000000000000000 ) ) ;
#4302 = VERTEX_POINT ( 'NONE', #4052 ) ;
#4303 = TOROIDAL_SURFACE ( 'NONE', #6700, 24.99999999999999645, 5.000000000000000000 ) ;
#4304 = DIRECTION ( 'NONE',  ( 1.224646799147353454E-16, 0.000000000000000000, -1.000000000000000000 ) ) ;
#4305 = FACE_OUTER_BOUND ( 'NONE', #3188, .T. ) ;
#4306 = ORIENTED_EDGE ( 'NONE', *, *, #2496, .F. ) ;
#4307 = CARTESIAN_POINT ( 'NONE',  ( 0.000000000000000000, 127.0000000000000000, 0.000000000000000000 ) ) ;
#4308 = DIRECTION ( 'NONE',  ( -0.000000000000000000, -1.000000000000000000, -0.000000000000000000 ) ) ;
#4309 = ORIENTED_EDGE ( 'NONE', *, *, #6724, .T. ) ;
#4310 = DIRECTION ( 'NONE',  ( -1.000000000000000000, 0.000000000000000000, 0.000000000000000000 ) ) ;
#4311 = CARTESIAN_POINT ( 'NONE',  ( 71.17928254424890611, 16.69380110197859324, 23.82724229592415810 ) ) ;
#4312 = AXIS2_PLACEMENT_3D ( 'NONE', #2700, #3459, #4514 ) ;
#4313 = VERTEX_POINT ( 'NONE', #9829 ) ;
#4314 = CARTESIAN_POINT ( 'NONE',  ( 77.29385721799278031, 15.00000000000008704, 20.32108911529004303 ) ) ;
#4315 = DIRECTION ( 'NONE',  ( 0.000000000000000000, 1.000000000000000000, 0.000000000000000000 ) ) ;
#4316 = VERTEX_POINT ( 'NONE', #4163 ) ;
#4317 = CARTESIAN_POINT ( 'NONE',  ( 0.000000000000000000, 110.0000000000000000, 3.250000000000000444 ) ) ;
#4318 = CARTESIAN_POINT ( 'NONE',  ( 70.75727862648629696, 47.58309759777085901, 24.86906317558853630 ) ) ;
#4319 = ORIENTED_EDGE ( 'NONE', *, *, #6863, .T. ) ;
#4320 = LINE ( 'NONE', #8116, #9597 ) ;
#4321 = FILL_AREA_STYLE_COLOUR ( '', #1321 ) ;
#4322 = CARTESIAN_POINT ( 'NONE',  ( -1.915364268218909816, 112.9374999986344079, -1.915364268218909150 ) ) ;
#4323 = ADVANCED_FACE ( 'NONE', ( #1791 ), #10077, .T. ) ;
#4324 = ORIENTED_EDGE ( 'NONE', *, *, #12003, .T. ) ;
#4325 = VERTEX_POINT ( 'NONE', #11214 ) ;
#4326 = ORIENTED_EDGE ( 'NONE', *, *, #11083, .F. ) ;
#4327 = DIRECTION ( 'NONE',  ( 0.000000000000000000, -0.000000000000000000, 1.000000000000000000 ) ) ;
#4328 = LINE ( 'NONE', #9116, #8318 ) ;
#4329 = ADVANCED_FACE ( 'NONE', ( #2545 ), #616, .F. ) ;
#4330 = CARTESIAN_POINT ( 'NONE',  ( 30.55518048406710818, 80.37544454677752981, 1.186187415305626436 ) ) ;
#4331 = CARTESIAN_POINT ( 'NONE',  ( -8.000000000000000000, 165.0000000000000000, -5.999999999999998224 ) ) ;
#4332 = CARTESIAN_POINT ( 'NONE',  ( -14.19078112930532853, 30.16666666668764307, 80.00000048127353125 ) ) ;
#4333 = DIRECTION ( 'NONE',  ( 0.000000000000000000, 0.000000000000000000, -1.000000000000000000 ) ) ;
#4334 = VECTOR ( 'NONE', #4925, 1000.000000000000000 ) ;
#4335 = CARTESIAN_POINT ( 'NONE',  ( 74.16198487095665826, 40.00000000000009237, -25.00000000000000000 ) ) ;
#4336 = FACE_OUTER_BOUND ( 'NONE', #10270, .T. ) ;
#4337 = B_SPLINE_CURVE_WITH_KNOTS ( 'NONE', 3,
 ( #12079, #7270, #11132, #2589 ),
 .UNSPECIFIED., .F., .F.,
 ( 4, 4 ),
 ( 0.0002502309401078032310, 0.0005002309401076767640 ),
 .UNSPECIFIED. ) ;
#4338 = CARTESIAN_POINT ( 'NONE',  ( 1.121994411437818862, 112.4999999986344079, 2.708734125000000326 ) ) ;
#4339 = CARTESIAN_POINT ( 'NONE',  ( -2.708734125000000326, 111.1249999986343937, -1.121994411437818195 ) ) ;
#4340 = CARTESIAN_POINT ( 'NONE',  ( -5.974274778359230709, 38.78525403784446723, 79.50000000000000000 ) ) ;
#4341 = EDGE_CURVE ( 'NONE', #11487, #3231, #11282, .T. ) ;
#4342 = AXIS2_PLACEMENT_3D ( 'NONE', #3767, #7512, #11322 ) ;
#4343 = ORIENTED_EDGE ( 'NONE', *, *, #6771, .F. ) ;
#4344 = CARTESIAN_POINT ( 'NONE',  ( 28.52887280570638495, 85.15789473684209554, 9.723794007404251261 ) ) ;
#4345 = ORIENTED_EDGE ( 'NONE', *, *, #5273, .T. ) ;
#4346 = DIRECTION ( 'NONE',  ( 0.000000000000000000, 0.000000000000000000, 1.000000000000000000 ) ) ;
#4347 = CARTESIAN_POINT ( 'NONE',  ( 89.80805993797383735, 275.0000000000000000, 71.82974571984303225 ) ) ;
#4348 = ORIENTED_EDGE ( 'NONE', *, *, #7430, .T. ) ;
#4349 = DIRECTION ( 'NONE',  ( 1.000000000000000000, 0.000000000000000000, 0.000000000000000000 ) ) ;
#4350 = CYLINDRICAL_SURFACE ( 'NONE', #12147, 3.250000000000000444 ) ;
#4351 = ORIENTED_EDGE ( 'NONE', *, *, #5560, .T. ) ;
#4352 = CARTESIAN_POINT ( 'NONE',  ( 72.61843774138907293, 50.00000000000000000, -18.75000000000000000 ) ) ;
#4353 = EDGE_CURVE ( 'NONE', #7098, #11714, #11656, .T. ) ;
#4354 = EDGE_CURVE ( 'NONE', #5087, #5348, #294, .T. ) ;
#4355 = ORIENTED_EDGE ( 'NONE', *, *, #11919, .T. ) ;
#4356 = DIRECTION ( 'NONE',  ( 1.000000000000000000, 0.000000000000000000, 0.000000000000000000 ) ) ;
#4357 = VECTOR ( 'NONE', #2167, 1000.000000000000000 ) ;
#4358 = FACE_BOUND ( 'NONE', #9792, .T. ) ;
#4359 = ORIENTED_EDGE ( 'NONE', *, *, #9902, .T. ) ;
#4360 = AXIS2_PLACEMENT_3D ( 'NONE', #2471, #12139, #12202 ) ;
#4361 = ORIENTED_EDGE ( 'NONE', *, *, #6169, .T. ) ;
#4362 = DIRECTION ( 'NONE',  ( 0.000000000000000000, 0.000000000000000000, 1.000000000000000000 ) ) ;
#4363 = CARTESIAN_POINT ( 'NONE',  ( 166.4644660940684275, 38.53553390593280881, 25.00000000000000000 ) ) ;
#4364 = VERTEX_POINT ( 'NONE', #9198 ) ;
#4365 = DIRECTION ( 'NONE',  ( 0.000000000000000000, 0.000000000000000000, 1.000000000000000000 ) ) ;
#4366 = CARTESIAN_POINT ( 'NONE',  ( 0.000000000000000000, 165.0000000000000000, 0.000000000000000000 ) ) ;
#4367 = CARTESIAN_POINT ( 'NONE',  ( 0.000000000000000000, 63.00000000000000000, -57.08203932499371547 ) ) ;
#4368 = ORIENTED_EDGE ( 'NONE', *, *, #408, .T. ) ;
#4369 = FACE_OUTER_BOUND ( 'NONE', #11067, .T. ) ;
#4370 = CARTESIAN_POINT ( 'NONE',  ( 76.84533340411822167, 15.12513703210600369, 21.12320159127833819 ) ) ;
#4371 = CIRCLE ( 'NONE', #3396, 5.000000000000004441 ) ;
#4372 = ADVANCED_BREP_SHAPE_REPRESENTATION ( '', ( #763, #1612 ), #10102 ) ;
#4373 = AXIS2_PLACEMENT_3D ( 'NONE', #8734, #198, #7811 ) ;
#4374 = ORIENTED_EDGE ( 'NONE', *, *, #10508, .T. ) ;
#4375 = CARTESIAN_POINT ( 'NONE',  ( 1.346194077712550063, 112.0624999972687590, 3.250000000000008438 ) ) ;
#4376 = CARTESIAN_POINT ( 'NONE',  ( 0.000000000000000000, 260.0000000000000000, 0.000000000000000000 ) ) ;
#4377 = ORIENTED_EDGE ( 'NONE', *, *, #10723, .T. ) ;
#4378 = CARTESIAN_POINT ( 'NONE',  ( 125.0000000000009663, 42.92893218813456713, -25.00000000000000000 ) ) ;
#4379 = CARTESIAN_POINT ( 'NONE',  ( 75.22303488722339182, 43.45724334910113384, 23.61575757524099117 ) ) ;
#4380 = EDGE_LOOP ( 'NONE', ( #233, #4374, #7693, #7848 ) ) ;
#4381 = DIRECTION ( 'NONE',  ( 0.000000000000000000, 0.000000000000000000, -1.000000000000000000 ) ) ;
#4382 = AXIS2_PLACEMENT_3D ( 'NONE', #199, #5013, #9793 ) ;
#4383 = CARTESIAN_POINT ( 'NONE',  ( -27.30107202361637775, 86.87046582918780757, -12.43589427268144831 ) ) ;
#4384 = CARTESIAN_POINT ( 'NONE',  ( -1.121994411437819084, 111.6249999986343937, 2.708734125000000326 ) ) ;
#4385 = SURFACE_SIDE_STYLE ('',( #11069 ) ) ;
#4386 = ORIENTED_EDGE ( 'NONE', *, *, #5546, .F. ) ;
#4387 = AXIS2_PLACEMENT_3D ( 'NONE', #8810, #6023, #2152 ) ;
#4388 = AXIS2_PLACEMENT_3D ( 'NONE', #9006, #7028, #11959 ) ;
#4389 = EDGE_CURVE ( 'NONE', #945, #8618, #4597, .T. ) ;
#4390 = UNCERTAINTY_MEASURE_WITH_UNIT (LENGTH_MEASURE( 1.000000000000000082E-05 ), #1532, 'distance_accuracy_value', 'NONE');
#4391 = DIRECTION ( 'NONE',  ( -0.000000000000000000, -1.000000000000000000, -0.000000000000000000 ) ) ;
#4392 = EDGE_CURVE ( 'NONE', #2926, #7629, #4792, .T. ) ;
#4393 = CARTESIAN_POINT ( 'NONE',  ( 25.00000000000000000, 445.0000000000000568, -59.99999999999999289 ) ) ;
#4394 = CARTESIAN_POINT ( 'NONE',  ( -30.98881549816775660, 77.00000000000001421, 6.657310619789788220 ) ) ;
#4395 = CARTESIAN_POINT ( 'NONE',  ( -107.1104145097476987, 275.0000000000000000, 41.86118851095882576 ) ) ;
#4396 = CARTESIAN_POINT ( 'NONE',  ( -32.21610632499845650, 86.34645847305816346, -9.037576414350890985 ) ) ;
#4397 = AXIS2_PLACEMENT_3D ( 'NONE', #1192, #1250, #3994 ) ;
#4398 = CARTESIAN_POINT ( 'NONE',  ( 30.63265341208206038, 76.40790137508867019, -5.685798939282528330 ) ) ;
#4399 = CARTESIAN_POINT ( 'NONE',  ( 10.46236448685246856, 20.50957335928671199, 74.26939691374536778 ) ) ;
#4400 = LINE ( 'NONE', #8195, #7063 ) ;
#4401 = CARTESIAN_POINT ( 'NONE',  ( 3.250000000000000444, 114.0000000000000000, 0.000000000000000000 ) ) ;
#4402 = CARTESIAN_POINT ( 'NONE',  ( -12.57411137850301763, 23.71650635094618664, 80.00000000000000000 ) ) ;
#4403 = AXIS2_PLACEMENT_3D ( 'NONE', #9970, #2558, #4304 ) ;
#4404 = VECTOR ( 'NONE', #9001, 1000.000000000000114 ) ;
#4405 = EDGE_CURVE ( 'NONE', #7080, #8555, #10646, .T. ) ;
#4406 = LINE ( 'NONE', #8445, #9176 ) ;
#4407 = ORIENTED_EDGE ( 'NONE', *, *, #6024, .T. ) ;
#4408 = CARTESIAN_POINT ( 'NONE',  ( 28.72281323269012532, 87.00000000000000000, 8.660254037844435260 ) ) ;
#4409 = VERTEX_POINT ( 'NONE', #10200 ) ;
#4410 = EDGE_CURVE ( 'NONE', #1153, #6351, #804, .T. ) ;
#4411 = CARTESIAN_POINT ( 'NONE',  ( -7.690781129305457320, 18.74166975080245834, 80.00000000000000000 ) ) ;
#4412 = CARTESIAN_POINT ( 'NONE',  ( 1.346194077712578041, 113.6874999972688300, -3.249999999999981792 ) ) ;
#4413 = EDGE_LOOP ( 'NONE', ( #2495, #2393, #8521, #1334, #11816 ) ) ;
#4414 = CYLINDRICAL_SURFACE ( 'NONE', #11647, 5.000000000000004441 ) ;
#4415 = VECTOR ( 'NONE', #4708, 1000.000000000000227 ) ;
#4416 = CARTESIAN_POINT ( 'NONE',  ( 0.000000000000000000, 110.0000000000000000, 0.000000000000000000 ) ) ;
#4417 = ORIENTED_EDGE ( 'NONE', *, *, #10512, .F. ) ;
#4418 = FACE_OUTER_BOUND ( 'NONE', #3537, .T. ) ;
#4419 = EDGE_CURVE ( 'NONE', #6910, #4839, #11147, .T. ) ;
#4420 = EDGE_CURVE ( 'NONE', #8153, #6043, #12254, .T. ) ;
#4421 = EDGE_LOOP ( 'NONE', ( #391, #9636, #6136, #5232 ) ) ;
#4422 = VECTOR ( 'NONE', #8526, 1000.000000000000000 ) ;
#4423 = CARTESIAN_POINT ( 'NONE',  ( 30.03968734988933420, 77.39454232463201322, -4.824121477407818048 ) ) ;
#4424 = DIRECTION ( 'NONE',  ( 0.000000000000000000, 1.000000000000000000, 0.000000000000000000 ) ) ;
#4425 = ORIENTED_EDGE ( 'NONE', *, *, #12198, .T. ) ;
#4426 = FACE_OUTER_BOUND ( 'NONE', #9300, .T. ) ;
#4427 = FACE_OUTER_BOUND ( 'NONE', #2565, .T. ) ;
#4428 = VERTEX_POINT ( 'NONE', #11967 ) ;
#4429 = DIRECTION ( 'NONE',  ( 0.000000000000000000, 0.000000000000000000, 1.000000000000000000 ) ) ;
#4430 = DIRECTION ( 'NONE',  ( -1.000000000000000000, 0.000000000000000000, -0.000000000000000000 ) ) ;
#4431 = LINE ( 'NONE', #5314, #10493 ) ;
#4432 = DIRECTION ( 'NONE',  ( 0.000000000000000000, 0.5000000000000011102, 0.8660254037844379305 ) ) ;
#4433 = VERTEX_POINT ( 'NONE', #6415 ) ;
#4434 = DIRECTION ( 'NONE',  ( 0.000000000000000000, 0.000000000000000000, 1.000000000000000000 ) ) ;
#4435 = VECTOR ( 'NONE', #817, 1000.000000000000000 ) ;
#4436 = DIRECTION ( 'NONE',  ( 0.000000000000000000, 0.000000000000000000, -1.000000000000000000 ) ) ;
#4437 = ORIENTED_EDGE ( 'NONE', *, *, #196, .T. ) ;
#4438 = DIRECTION ( 'NONE',  ( 0.000000000000000000, 0.000000000000000000, 1.000000000000000000 ) ) ;
#4439 = CARTESIAN_POINT ( 'NONE',  ( -7.907287480251421030, 41.13333024919781167, 79.50000000000000000 ) ) ;
#4440 = ORIENTED_EDGE ( 'NONE', *, *, #11628, .F. ) ;
#4441 = LINE ( 'NONE', #11937, #483 ) ;
#4442 = CARTESIAN_POINT ( 'NONE',  ( -23.42809864819168553, 58.42809864819167132, 66.05997777686947359 ) ) ;
#4443 = VECTOR ( 'NONE', #8068, 1000.000000000000000 ) ;
#4444 = ORIENTED_EDGE ( 'NONE', *, *, #6773, .T. ) ;
#4445 = LINE ( 'NONE', #583, #12271 ) ;
#4446 = ADVANCED_FACE ( 'NONE', ( #1674 ), #10839, .T. ) ;
#4447 = DIRECTION ( 'NONE',  ( 0.8660254037844397068, 0.4999999999999981681, 0.000000000000000000 ) ) ;
#4448 = CARTESIAN_POINT ( 'NONE',  ( 3.249999999999999556, 114.8124999972688016, -1.346194077712561166 ) ) ;
#4449 = CARTESIAN_POINT ( 'NONE',  ( -1.346194077712560944, 114.5624999972688300, -3.249999999999999556 ) ) ;
#4450 = ADVANCED_FACE ( 'NONE', ( #10321 ), #9321, .F. ) ;
#4451 = EDGE_LOOP ( 'NONE', ( #8123, #673, #10360, #1647 ) ) ;
#4452 = ORIENTED_EDGE ( 'NONE', *, *, #7641, .T. ) ;
#4453 = FILL_AREA_STYLE ('',( #657 ) ) ;
#4454 = AXIS2_PLACEMENT_3D ( 'NONE', #11106, #3623, #4676 ) ;
#4455 = FACE_BOUND ( 'NONE', #9008, .T. ) ;
#4456 = CARTESIAN_POINT ( 'NONE',  ( -69.85388127645428824, 17.99999999999971223, -31.17691453623957543 ) ) ;
#4457 = CARTESIAN_POINT ( 'NONE',  ( 0.000000000000000000, 127.0000000000000000, -15.00000000000000000 ) ) ;
#4458 = CARTESIAN_POINT ( 'NONE',  ( -7.474274778359196070, 18.61666975080236597, 80.00000000000000000 ) ) ;
#4459 = CARTESIAN_POINT ( 'NONE',  ( 5.092712519748452848, 41.38333024919784719, 79.50000000000000000 ) ) ;
#4460 = CARTESIAN_POINT ( 'NONE',  ( 0.000000000000000000, 122.5000000000000000, -10.49999999999999822 ) ) ;
#4461 = EDGE_CURVE ( 'NONE', #5322, #8932, #549, .T. ) ;
#4462 = DIRECTION ( 'NONE',  ( -1.000000000000000000, 0.000000000000000000, -1.224646799147352961E-16 ) ) ;
#4463 = DIRECTION ( 'NONE',  ( 0.000000000000000000, 1.000000000000000000, 0.000000000000000000 ) ) ;
#4464 = ORIENTED_EDGE ( 'NONE', *, *, #9238, .F. ) ;
#4465 = AXIS2_PLACEMENT_3D ( 'NONE', #11776, #11837, #4155 ) ;
#4466 = CARTESIAN_POINT ( 'NONE',  ( 3.249999999999999556, 110.9374999999999858, -1.346194077712561610 ) ) ;
#4467 = LINE ( 'NONE', #8384, #6386 ) ;
#4468 = EDGE_CURVE ( 'NONE', #11813, #7928, #8391, .T. ) ;
#4469 = CIRCLE ( 'NONE', #9239, 12.99999999999999822 ) ;
#4470 = DIRECTION ( 'NONE',  ( 1.224646799147354193E-16, 0.000000000000000000, -1.000000000000000000 ) ) ;
#4471 = CONICAL_SURFACE ( 'NONE', #11455, 2.099999999999998312, 1.029744258676656532 ) ;
#4472 = ORIENTED_EDGE ( 'NONE', *, *, #2892, .F. ) ;
#4473 = CARTESIAN_POINT ( 'NONE',  ( 0.000000000000000000, 216.0365690573663926, 0.000000000000000000 ) ) ;
#4474 = CARTESIAN_POINT ( 'NONE',  ( -7.762949912955313891, 18.78333641746978699, 80.00000000000000000 ) ) ;
#4475 = LINE ( 'NONE', #1675, #10465 ) ;
#4476 = ORIENTED_EDGE ( 'NONE', *, *, #8878, .F. ) ;
#4477 = LINE ( 'NONE', #7531, #6653 ) ;
#4478 = CARTESIAN_POINT ( 'NONE',  ( 170.0000000000011369, 35.00000000000004974, 25.00000000000000000 ) ) ;
#4479 = EDGE_CURVE ( 'NONE', #5668, #5619, #11090, .T. ) ;
#4480 = AXIS2_PLACEMENT_3D ( 'NONE', #6030, #470, #11648 ) ;
#4481 = ORIENTED_EDGE ( 'NONE', *, *, #2746, .F. ) ;
#4482 = DIRECTION ( 'NONE',  ( -0.000000000000000000, -1.000000000000000000, -0.000000000000000000 ) ) ;
#4483 = AXIS2_PLACEMENT_3D ( 'NONE', #11417, #10656, #9709 ) ;
#4484 = EDGE_LOOP ( 'NONE', ( #2365, #11020, #10902, #3633 ) ) ;
#4485 = ORIENTED_EDGE ( 'NONE', *, *, #6327, .F. ) ;
#4486 = LINE ( 'NONE', #11034, #7124 ) ;
#4487 = CARTESIAN_POINT ( 'NONE',  ( 25.00000000000000000, 445.0000000000000568, -90.00000000000000000 ) ) ;
#4488 = ORIENTED_EDGE ( 'NONE', *, *, #7328, .F. ) ;
#4489 = AXIS2_PLACEMENT_3D ( 'NONE', #8451, #3973, #4658 ) ;
#4490 =( BOUNDED_CURVE ( )  B_SPLINE_CURVE ( 2, ( #7072, #5150, #8928, #398, #9928, #10625, #7933, #5025, #6828 ),
 .UNSPECIFIED., .F., .F. ) 
 B_SPLINE_CURVE_WITH_KNOTS ( ( 3, 2, 2, 2, 3 ),
 ( 0.3125000000000002776, 0.3437500000000003331, 0.3750000000000003331, 0.4062500000000003331, 0.4375000000000003886 ),
 .UNSPECIFIED. ) 
 CURVE ( )  GEOMETRIC_REPRESENTATION_ITEM ( )  RATIONAL_B_SPLINE_CURVE ( ( 0.9999999999999993339, 0.9238795325112874046, 1.000000000000000000, 0.9238795325112867385, 1.000000000000000000, 0.9238795325112867385, 1.000000000000000000, 0.9238795325112857393, 1.000000000000000888 ) ) 
 REPRESENTATION_ITEM ( '' )  );
#4491 = CARTESIAN_POINT ( 'NONE',  ( -1.440781129305471087, 43.00000000000008527, 79.50000000000000000 ) ) ;
#4492 = CARTESIAN_POINT ( 'NONE',  ( 2.500000000000000000, 2.357898499370431722, -2.818925648462311528E-15 ) ) ;
#4493 = ORIENTED_EDGE ( 'NONE', *, *, #5646, .F. ) ;
#4494 = ADVANCED_FACE ( 'NONE', ( #6289 ), #9133, .T. ) ;
#4495 = DIRECTION ( 'NONE',  ( 1.000000000000000000, 0.000000000000000000, 0.000000000000000000 ) ) ;
#4496 = CLOSED_SHELL ( 'NONE', ( #8874, #1856, #6733, #11048, #225, #5932, #1394, #5933, #2805, #6413, #575, #9689, #2363, #11468, #11262, #61, #3687, #2063, #6333, #9974, #8429, #6819, #4045, #4521, #5506, #5288, #10288, #63, #52, #1716, #10098, #6457, #8244, #8140, #9876, #5475, #2465, #10042, #2817, #3897, #10570, #7705, #918, #8324, #11211, #1242, #5707, #1530, #10226, #4235, #10711, #6474, #477, #846, #1404, #282, #5416, #9251, #1483, #700, #8060, #11412, #8390, #4323, #11892, #5567, #10892, #6354, #3588, #1061, #5643, #6129, #863, #4714, #6408, #1151, #141, #8440, #1302, #1515, #6604, #2306, #3343 ) ) ;
#4497 = FACE_OUTER_BOUND ( 'NONE', #2635, .T. ) ;
#4498 = VECTOR ( 'NONE', #10653, 1000.000000000000000 ) ;
#4499 = DIRECTION ( 'NONE',  ( 0.000000000000000000, 1.000000000000000000, 0.000000000000000000 ) ) ;
#4500 = CARTESIAN_POINT ( 'NONE',  ( 1.990051048614449116E-16, 111.1249999972688158, 3.250000000000000444 ) ) ;
#4501 = ORIENTED_EDGE ( 'NONE', *, *, #1892, .T. ) ;
#4502 = CARTESIAN_POINT ( 'NONE',  ( 0.000000000000000000, 75.00000000000001421, 90.00000000000002842 ) ) ;
#4503 = DIRECTION ( 'NONE',  ( 0.4999999999999985012, -0.8660254037844394848, 0.000000000000000000 ) ) ;
#4504 = AXIS2_PLACEMENT_3D ( 'NONE', #3022, #11568, #7756 ) ;
#4505 = AXIS2_PLACEMENT_3D ( 'NONE', #1293, #5104, #6216 ) ;
#4506 = ORIENTED_EDGE ( 'NONE', *, *, #4468, .F. ) ;
#4507 = CARTESIAN_POINT ( 'NONE',  ( -16.19078112930547064, 30.00000000000008882, 78.00000000000000000 ) ) ;
#4508 = DIRECTION ( 'NONE',  ( 1.000000000000000000, 0.000000000000000000, -0.000000000000000000 ) ) ;
#4509 = ORIENTED_EDGE ( 'NONE', *, *, #7456, .F. ) ;
#4510 = DIRECTION ( 'NONE',  ( 0.7071067811865495711, 0.7071067811865455743, 0.000000000000000000 ) ) ;
#4511 = CARTESIAN_POINT ( 'NONE',  ( 0.000000000000000000, 122.0000000000000000, 0.000000000000000000 ) ) ;
#4512 = ORIENTED_EDGE ( 'NONE', *, *, #4773, .F. ) ;
#4513 = CARTESIAN_POINT ( 'NONE',  ( 150.0000000000010800, 15.00000000000008882, -19.99999999999999645 ) ) ;
#4514 = DIRECTION ( 'NONE',  ( 0.000000000000000000, 0.000000000000000000, 1.000000000000000000 ) ) ;
#4515 = DIRECTION ( 'NONE',  ( 0.000000000000000000, 0.000000000000000000, 1.000000000000000000 ) ) ;
#4516 = CARTESIAN_POINT ( 'NONE',  ( 2.708734124999999882, 113.6249999986344079, 1.121994411437818862 ) ) ;
#4517 = CIRCLE ( 'NONE', #740, 75.00000000000001421 ) ;
#4518 = EDGE_LOOP ( 'NONE', ( #3054, #11569, #2613, #5394 ) ) ;
#4519 =( NAMED_UNIT ( * ) PLANE_ANGLE_UNIT ( ) SI_UNIT ( $, .RADIAN. ) );
#4520 = EDGE_CURVE ( 'NONE', #7164, #11798, #10637, .T. ) ;
#4521 = ADVANCED_FACE ( 'NONE', ( #11336 ), #4916, .F. ) ;
#4522 = AXIS2_PLACEMENT_3D ( 'NONE', #8348, #4499, #8289 ) ;
#4523 = LINE ( 'NONE', #2646, #6051 ) ;
#4524 = FACE_OUTER_BOUND ( 'NONE', #11676, .T. ) ;
#4526 = ADVANCED_FACE ( 'NONE', ( #1919 ), #6672, .F. ) ;
#4525 = LINE ( 'NONE', #11266, #2641 ) ;
#4527 = CARTESIAN_POINT ( 'NONE',  ( 6.000000000000000888, 62.00000000000000000, 60.00000000000002132 ) ) ;
#4528 = DIRECTION ( 'NONE',  ( 0.000000000000000000, 1.000000000000000000, 0.000000000000000000 ) ) ;
#4529 = CARTESIAN_POINT ( 'NONE',  ( 0.000000000000000000, 50.00000000000000000, 0.000000000000000000 ) ) ;
#4530 = DIRECTION ( 'NONE',  ( 0.000000000000000000, 1.000000000000000000, -0.000000000000000000 ) ) ;
#4531 = CARTESIAN_POINT ( 'NONE',  ( -5.970153145843347347E-16, 110.7500000000000000, -3.250000000000000444 ) ) ;
#4532 = CARTESIAN_POINT ( 'NONE',  ( -30.07733313487553772, 77.00000000000709122, 4.660254037819535178 ) ) ;
#4533 = CARTESIAN_POINT ( 'NONE',  ( 3.592712519748626931, 21.21474596215575659, 80.00000000000000000 ) ) ;
#4534 = VERTEX_POINT ( 'NONE', #7650 ) ;
#4535 = DIRECTION ( 'NONE',  ( 0.000000000000000000, 0.000000000000000000, -1.000000000000000000 ) ) ;
#4536 = DIRECTION ( 'NONE',  ( 0.000000000000000000, 0.000000000000000000, 1.000000000000000000 ) ) ;
#4537 = EDGE_LOOP ( 'NONE', ( #11933, #1992, #485, #490 ) ) ;
#4538 = PLANE ( 'NONE',  #6265 ) ;
#4539 = DIRECTION ( 'NONE',  ( 0.000000000000000000, 0.000000000000000000, 1.000000000000000000 ) ) ;
#4540 = ORIENTED_EDGE ( 'NONE', *, *, #8707, .T. ) ;
#4541 = LINE ( 'NONE', #5613, #8548 ) ;
#4542 = VECTOR ( 'NONE', #7423, 1000.000000000000000 ) ;
#4543 = ORIENTED_EDGE ( 'NONE', *, *, #11154, .T. ) ;
#4544 = EDGE_CURVE ( 'NONE', #3229, #6205, #5728, .T. ) ;
#4545 = CARTESIAN_POINT ( 'NONE',  ( 34.72842983617974966, 77.03714026276665550, -8.681696978550554888 ) ) ;
#4547 = VERTEX_POINT ( 'NONE', #6654 ) ;
#4546 = CARTESIAN_POINT ( 'NONE',  ( 25.00000000000000000, 570.2996408614167194, -59.99999999999999289 ) ) ;
#4548 = EDGE_LOOP ( 'NONE', ( #6796, #9166 ) ) ;
#4549 = LINE ( 'NONE', #7364, #9565 ) ;
#4550 = FACE_OUTER_BOUND ( 'NONE', #1328, .T. ) ;
#4551 = VERTEX_POINT ( 'NONE', #1851 ) ;
#4553 = PRESENTATION_LAYER_ASSIGNMENT (  '', '', ( #10113 ) ) ;
#4552 = DIRECTION ( 'NONE',  ( 0.000000000000000000, 0.000000000000000000, 1.000000000000000000 ) ) ;
#4554 = LINE ( 'NONE', #8468, #3291 ) ;
#4555 = DIRECTION ( 'NONE',  ( -0.2500000000000003886, 6.938893903907242183E-16, 0.9682458365518542553 ) ) ;
#4556 = DIRECTION ( 'NONE',  ( 0.000000000000000000, 1.000000000000000000, 0.000000000000000000 ) ) ;
#4557 = ORIENTED_EDGE ( 'NONE', *, *, #11197, .F. ) ;
#4558 = CARTESIAN_POINT ( 'NONE',  ( 1.915364268218909150, 111.6874999986344079, 1.915364268218909150 ) ) ;
#4559 = LINE ( 'NONE', #2749, #8372 ) ;
#4560 = B_SPLINE_CURVE_WITH_KNOTS ( 'NONE', 3,
 ( #11829, #7082, #10881, #5462 ),
 .UNSPECIFIED., .F., .F.,
 ( 4, 4 ),
 ( 0.0002502309401077386667, 0.0005002309401076767640 ),
 .UNSPECIFIED. ) ;
#4561 = EDGE_CURVE ( 'NONE', #11110, #7233, #11457, .T. ) ;
#4562 = ORIENTED_EDGE ( 'NONE', *, *, #8620, .F. ) ;
#4563 = EDGE_CURVE ( 'NONE', #2554, #9087, #4781, .T. ) ;
#4564 = CARTESIAN_POINT ( 'NONE',  ( -1.274114462640252521, 17.00000000000009237, 80.00000000000000000 ) ) ;
#4565 = CARTESIAN_POINT ( 'NONE',  ( 72.02249449389091751, 49.73282098440206767, 20.92514131019473567 ) ) ;
#4566 = ORIENTED_EDGE ( 'NONE', *, *, #4224, .T. ) ;
#4567 = CARTESIAN_POINT ( 'NONE',  ( -12.57411137850301763, 23.71650635094618664, 80.00000000000000000 ) ) ;
#4568 = VERTEX_POINT ( 'NONE', #10577 ) ;
#4569 = DIRECTION ( 'NONE',  ( -0.000000000000000000, -1.000000000000000000, 0.000000000000000000 ) ) ;
#4570 = LINE ( 'NONE', #8365, #6391 ) ;
#4571 = CIRCLE ( 'NONE', #10333, 80.00000000000001421 ) ;
#4572 = CARTESIAN_POINT ( 'NONE',  ( 2.708734124999999882, 113.5624999986344079, 0.000000000000000000 ) ) ;
#4573 = CARTESIAN_POINT ( 'NONE',  ( 1.915364268218908705, 111.4374999986344079, -1.915364268218909594 ) ) ;
#4574 = VERTEX_POINT ( 'NONE', #8572 ) ;
#4575 = SURFACE_STYLE_FILL_AREA ( #4453 ) ;
#4576 = EDGE_CURVE ( 'NONE', #9884, #2552, #9175, .T. ) ;
#4577 = EDGE_CURVE ( 'NONE', #7882, #2552, #12334, .T. ) ;
#4578 = B_SPLINE_CURVE_WITH_KNOTS ( 'NONE', 3,
 ( #741, #610, #2481, #5477 ),
 .UNSPECIFIED., .F., .F.,
 ( 4, 4 ),
 ( 0.0009573067811865457882, 0.001207306781186546010 ),
 .UNSPECIFIED. ) ;
#4579 = VECTOR ( 'NONE', #11856, 1000.000000000000000 ) ;
#4580 = CARTESIAN_POINT ( 'NONE',  ( -7.907287480251413925, 18.86666975080236597, 79.50000000000000000 ) ) ;
#4581 = CARTESIAN_POINT ( 'NONE',  ( 0.000000000000000000, 67.00000000000000000, 0.000000000000000000 ) ) ;
#4582 = CARTESIAN_POINT ( 'NONE',  ( 142.0710678118665555, 59.99999999999997868, 20.00000000000000000 ) ) ;
#4583 = DIRECTION ( 'NONE',  ( -0.000000000000000000, -0.000000000000000000, 1.000000000000000000 ) ) ;
#4584 = CARTESIAN_POINT ( 'NONE',  ( -27.97213591028565460, 86.27509468223345834, -11.40681812415373209 ) ) ;
#4585 = DIRECTION ( 'NONE',  ( 0.000000000000000000, 0.000000000000000000, 1.000000000000000000 ) ) ;
#4586 = FACE_BOUND ( 'NONE', #7622, .T. ) ;
#4587 = ORIENTED_EDGE ( 'NONE', *, *, #11781, .F. ) ;
#4588 = CARTESIAN_POINT ( 'NONE',  ( 3.250000000000000444, 111.0000000000000000, 0.000000000000000000 ) ) ;
#4589 = VECTOR ( 'NONE', #5489, 1000.000000000000000 ) ;
#4590 = CARTESIAN_POINT ( 'NONE',  ( 0.000000000000000000, 290.0000000000000568, 0.000000000000000000 ) ) ;
#4591 = CIRCLE ( 'NONE', #404, 70.00000000000001421 ) ;
#4592 = CARTESIAN_POINT ( 'NONE',  ( 0.9400506840132951680, 15.12220259995254779, 75.00000000000001421 ) ) ;
#4593 = ORIENTED_EDGE ( 'NONE', *, *, #5030, .F. ) ;
#4594 = VECTOR ( 'NONE', #5764, 1000.000000000000114 ) ;
#4595 = VECTOR ( 'NONE', #4503, 1000.000000000000114 ) ;
#4596 = LINE ( 'NONE', #11145, #2456 ) ;
#4597 = LINE ( 'NONE', #676, #1298 ) ;
#4598 = CARTESIAN_POINT ( 'NONE',  ( 69.52686081700198883, 19.32205100516523899, -28.12499999881303836 ) ) ;
#4599 = ORIENTED_EDGE ( 'NONE', *, *, #10451, .F. ) ;
#4600 = CARTESIAN_POINT ( 'NONE',  ( 4.025725221640849227, 21.46474596215575659, 80.00000000000000000 ) ) ;
#4601 = EDGE_CURVE ( 'NONE', #334, #2134, #9445, .T. ) ;
#4602 = DIRECTION ( 'NONE',  ( 0.000000000000000000, 0.000000000000000000, 1.000000000000000000 ) ) ;
#4603 = CIRCLE ( 'NONE', #2413, 14.99999999999999822 ) ;
#4604 = ORIENTED_EDGE ( 'NONE', *, *, #5572, .T. ) ;
#4605 = DIRECTION ( 'NONE',  ( -0.000000000000000000, -0.000000000000000000, 1.000000000000000000 ) ) ;
#4606 = AXIS2_PLACEMENT_3D ( 'NONE', #9725, #5010, #9607 ) ;
#4607 = ORIENTED_EDGE ( 'NONE', *, *, #7404, .F. ) ;
#4608 = AXIS2_PLACEMENT_3D ( 'NONE', #11645, #8816, #6092 ) ;
#4609 = DIRECTION ( 'NONE',  ( 0.000000000000000000, 1.000000000000000000, 0.000000000000000000 ) ) ;
#4611 = ORIENTED_EDGE ( 'NONE', *, *, #6267, .F. ) ;
#4610 = DIRECTION ( 'NONE',  ( -0.000000000000000000, 0.8660254037844402619, 0.4999999999999975575 ) ) ;
#4612 = ORIENTED_EDGE ( 'NONE', *, *, #597, .F. ) ;
#4613 = CYLINDRICAL_SURFACE ( 'NONE', #5511, 75.00000000000002842 ) ;
#4614 = ORIENTED_EDGE ( 'NONE', *, *, #8890, .T. ) ;
#4615 = DIRECTION ( 'NONE',  ( 1.000000000000000000, 0.000000000000000000, 0.000000000000000000 ) ) ;
#4616 = CARTESIAN_POINT ( 'NONE',  ( 0.000000000000000000, 87.00000000000000000, 0.000000000000000000 ) ) ;
#4617 = FACE_OUTER_BOUND ( 'NONE', #10323, .T. ) ;
#4618 = DIRECTION ( 'NONE',  ( 0.000000000000000000, 1.000000000000000000, -0.000000000000000000 ) ) ;
#4619 = ORIENTED_EDGE ( 'NONE', *, *, #7342, .T. ) ;
#4620 = CARTESIAN_POINT ( 'NONE',  ( 2.708734124999999437, 113.4999999986344079, -1.121994411437820638 ) ) ;
#4621 = EDGE_CURVE ( 'NONE', #6185, #10487, #8699, .T. ) ;
#4622 = LINE ( 'NONE', #5509, #1225 ) ;
#4623 = EDGE_CURVE ( 'NONE', #11632, #6660, #3688, .T. ) ;
#4624 = VECTOR ( 'NONE', #9371, 1000.000000000000000 ) ;
#4625 = EDGE_LOOP ( 'NONE', ( #9747, #529, #9005, #4999, #324, #2638, #6306, #9540, #7157, #7425, #2116, #8824 ) ) ;
#4626 = PLANE ( 'NONE',  #385 ) ;
#4627 = CARTESIAN_POINT ( 'NONE',  ( -15.97595206614365182, 27.41870735413941773, 73.27878722613796469 ) ) ;
#4628 = ORIENTED_EDGE ( 'NONE', *, *, #597, .T. ) ;
#4629 = DIRECTION ( 'NONE',  ( -0.5000000000000006661, -0.8660254037844383745, 0.000000000000000000 ) ) ;
#4630 = DIRECTION ( 'NONE',  ( 0.000000000000000000, 0.000000000000000000, 1.000000000000000000 ) ) ;
#4631 = ORIENTED_EDGE ( 'NONE', *, *, #5168, .T. ) ;
#4632 = LINE ( 'NONE', #6324, #4923 ) ;
#4633 = CARTESIAN_POINT ( 'NONE',  ( 0.000000000000000000, 5.000000000000129674, 0.000000000000000000 ) ) ;
#4634 = CIRCLE ( 'NONE', #11614, 95.00000000000002842 ) ;
#4635 = CARTESIAN_POINT ( 'NONE',  ( -2.708734124999999882, 113.9999999986343937, 1.121994411437818862 ) ) ;
#4636 = EDGE_CURVE ( 'NONE', #6043, #5183, #3849, .T. ) ;
#4637 = EDGE_CURVE ( 'NONE', #6351, #7137, #6480, .T. ) ;
#4638 = DIRECTION ( 'NONE',  ( -0.000000000000000000, -1.000000000000000000, -0.000000000000000000 ) ) ;
#4639 = VERTEX_POINT ( 'NONE', #7587 ) ;
#4640 = B_SPLINE_CURVE_WITH_KNOTS ( 'NONE', 3,
 ( #1108, #4779, #226, #9753, #4914, #9569, #8697, #3970, #12333, #3783 ),
 .UNSPECIFIED., .F., .F.,
 ( 4, 2, 2, 2, 4 ),
 ( 2.797157557069881010E-17, 0.001173140257025584660, 0.002346280514051141131, 0.003519420771076697818, 0.004692561028102254506 ),
 .UNSPECIFIED. ) ;
#4641 = VECTOR ( 'NONE', #6792, 1000.000000000000000 ) ;
#4642 = DIRECTION ( 'NONE',  ( 0.000000000000000000, 0.000000000000000000, 1.000000000000000000 ) ) ;
#4643 = CARTESIAN_POINT ( 'NONE',  ( 116.4243635975512490, 275.0000000000000000, 45.50129185973946022 ) ) ;
#4644 = ORIENTED_EDGE ( 'NONE', *, *, #5415, .F. ) ;
#4645 = DIRECTION ( 'NONE',  ( -0.000000000000000000, -1.000000000000000000, -0.000000000000000000 ) ) ;
#4646 = CYLINDRICAL_SURFACE ( 'NONE', #2797, 17.00000000000000000 ) ;
#4647 = DIRECTION ( 'NONE',  ( -0.000000000000000000, -1.000000000000000000, -0.000000000000000000 ) ) ;
#4648 = CARTESIAN_POINT ( 'NONE',  ( -7.907287480251421030, 41.13333024919781167, 79.50000000000000000 ) ) ;
#4649 = EDGE_CURVE ( 'NONE', #11984, #11751, #9631, .T. ) ;
#4650 = VERTEX_POINT ( 'NONE', #11588 ) ;
#4651 = VECTOR ( 'NONE', #2400, 1000.000000000000000 ) ;
#4652 = DIRECTION ( 'NONE',  ( 0.000000000000000000, -1.000000000000000000, 0.000000000000000000 ) ) ;
#4653 = DIRECTION ( 'NONE',  ( 0.000000000000000000, 0.000000000000000000, 1.000000000000000000 ) ) ;
#4654 = DIRECTION ( 'NONE',  ( 0.000000000000000000, 1.000000000000000000, 0.000000000000000000 ) ) ;
#4655 = ORIENTED_EDGE ( 'NONE', *, *, #2233, .T. ) ;
#4656 = CARTESIAN_POINT ( 'NONE',  ( 8.809218870694669690, 29.75000000000019540, 79.50000000000000000 ) ) ;
#4657 = AXIS2_PLACEMENT_3D ( 'NONE', #6522, #5649, #6576 ) ;
#4658 = DIRECTION ( 'NONE',  ( 0.000000000000000000, 0.000000000000000000, 1.000000000000000000 ) ) ;
#4659 = CARTESIAN_POINT ( 'NONE',  ( 0.000000000000000000, 50.00000000000000000, 0.000000000000000000 ) ) ;
#4660 = ORIENTED_EDGE ( 'NONE', *, *, #8369, .F. ) ;
#4661 = CARTESIAN_POINT ( 'NONE',  ( 145.0000000000011369, 225.0000000000000853, 25.00000000000000000 ) ) ;
#4662 = DIRECTION ( 'NONE',  ( 0.000000000000000000, 1.000000000000000000, 0.000000000000000000 ) ) ;
#4663 = ORIENTED_EDGE ( 'NONE', *, *, #9564, .T. ) ;
#4664 = CYLINDRICAL_SURFACE ( 'NONE', #1400, 5.000000000000000888 ) ;
#4665 = AXIS2_PLACEMENT_3D ( 'NONE', #9386, #8454, #10080 ) ;
#4666 = EDGE_CURVE ( 'NONE', #3422, #11988, #6593, .T. ) ;
#4667 = ORIENTED_EDGE ( 'NONE', *, *, #7495, .T. ) ;
#4668 = EDGE_CURVE ( 'NONE', #5411, #2246, #7076, .T. ) ;
#4669 = CARTESIAN_POINT ( 'NONE',  ( 5.092712519748611832, 18.61666975080242992, 80.00000000000000000 ) ) ;
#4670 = CARTESIAN_POINT ( 'NONE',  ( -69.85388127645428824, 79.49999999999998579, 4.330127018922231841 ) ) ;
#4671 = ORIENTED_EDGE ( 'NONE', *, *, #4520, .F. ) ;
#4672 = FACE_OUTER_BOUND ( 'NONE', #10726, .T. ) ;
#4673 = ORIENTED_EDGE ( 'NONE', *, *, #7241, .T. ) ;
#4674 = ADVANCED_FACE ( 'NONE', ( #5161 ), #4095, .F. ) ;
#4675 = CIRCLE ( 'NONE', #11050, 25.00000000000000000 ) ;
#4676 = DIRECTION ( 'NONE',  ( 0.4999999999999919509, 0.000000000000000000, 0.8660254037844432595 ) ) ;
#4677 = CIRCLE ( 'NONE', #10647, 10.49999999999999822 ) ;
#4678 = CARTESIAN_POINT ( 'NONE',  ( 0.000000000000000000, 115.0000000000000000, 0.000000000000000000 ) ) ;
#4679 = FACE_OUTER_BOUND ( 'NONE', #10710, .T. ) ;
#4680 = ORIENTED_EDGE ( 'NONE', *, *, #5783, .T. ) ;
#4681 = CARTESIAN_POINT ( 'NONE',  ( -2.708734124999999882, 113.0624999986344079, 3.317242575922456639E-16 ) ) ;
#4682 = PLANE ( 'NONE',  #217 ) ;
#4683 = CIRCLE ( 'NONE', #6882, 17.00000000000000000 ) ;
#4684 = ORIENTED_EDGE ( 'NONE', *, *, #8884, .F. ) ;
#4685 = LINE ( 'NONE', #11306, #206 ) ;
#4686 = DIRECTION ( 'NONE',  ( 1.000000000000000000, 0.000000000000000000, 0.000000000000000000 ) ) ;
#4687 = ORIENTED_EDGE ( 'NONE', *, *, #510, .F. ) ;
#4688 = CARTESIAN_POINT ( 'NONE',  ( 32.18413411689675030, 86.41755723128771649, 8.996527527148016290 ) ) ;
#4689 = ORIENTED_EDGE ( 'NONE', *, *, #8117, .T. ) ;
#4690 = DIRECTION ( 'NONE',  ( 0.000000000000000000, 1.000000000000000000, 0.000000000000000000 ) ) ;
#4691 = CARTESIAN_POINT ( 'NONE',  ( -0.9407811293052614765, 20.00000000000009237, 80.00000000000000000 ) ) ;
#4692 = VECTOR ( 'NONE', #6564, 1000.000000000000000 ) ;
#4693 = CARTESIAN_POINT ( 'NONE',  ( 1.915364268218909150, 111.6874999986344079, 1.915364268218909150 ) ) ;
#4694 = PLANE ( 'NONE',  #8860 ) ;
#4695 = VERTEX_POINT ( 'NONE', #5223 ) ;
#4696 = SHAPE_DEFINITION_REPRESENTATION ( #2110, #3713 ) ;
#4697 = VECTOR ( 'NONE', #2121, 1000.000000000000000 ) ;
#4698 = EDGE_CURVE ( 'NONE', #5363, #11844, #9816, .T. ) ;
#4699 = VERTEX_POINT ( 'NONE', #7088 ) ;
#4700 = LINE ( 'NONE', #848, #12027 ) ;
#4701 = DIRECTION ( 'NONE',  ( 1.000000000000000000, 0.000000000000000000, 0.000000000000000000 ) ) ;
#4702 = ORIENTED_EDGE ( 'NONE', *, *, #5259, .F. ) ;
#4703 = EDGE_CURVE ( 'NONE', #9396, #4409, #4037, .T. ) ;
#4704 = CARTESIAN_POINT ( 'NONE',  ( 1.224646799147353059E-15, 115.0000000000000000, 9.999999999999998224 ) ) ;
#4705 = CARTESIAN_POINT ( 'NONE',  ( -14.19078112930532853, 30.25000000000008882, 79.50000000000000000 ) ) ;
#4706 = CIRCLE ( 'NONE', #5309, 75.00000000000001421 ) ;
#4707 = CARTESIAN_POINT ( 'NONE',  ( 17.30235457177317571, 285.0000000000000568, -113.6909342308024407 ) ) ;
#4708 = DIRECTION ( 'NONE',  ( -0.8660254037844385966, 0.5000000000000000000, 0.000000000000000000 ) ) ;
#4709 = MANIFOLD_SOLID_BREP ( 'Extrude-Thin3', #1313 ) ;
#4710 = ORIENTED_EDGE ( 'NONE', *, *, #4838, .F. ) ;
#4711 = FACE_OUTER_BOUND ( 'NONE', #8267, .T. ) ;
#4712 = CIRCLE ( 'NONE', #2925, 4.250000000000000000 ) ;
#4713 = EDGE_CURVE ( 'NONE', #4212, #10899, #4973, .T. ) ;
#4714 = ADVANCED_FACE ( 'NONE', ( #6094 ), #286, .T. ) ;
#4715 = CARTESIAN_POINT ( 'NONE',  ( 74.52821641976538558, 42.10288043194585583, -24.53929266990226665 ) ) ;
#4716 = PRESENTATION_STYLE_ASSIGNMENT (( #11521 ) ) ;
#4717 = ORIENTED_EDGE ( 'NONE', *, *, #6724, .F. ) ;
#4718 = CARTESIAN_POINT ( 'NONE',  ( 0.000000000000000000, 216.0365690573663926, 0.000000000000000000 ) ) ;
#4719 = DIRECTION ( 'NONE',  ( 1.000000000000000000, 0.000000000000000000, 0.000000000000000000 ) ) ;
#4720 = CARTESIAN_POINT ( 'NONE',  ( 69.91894869711104832, 15.48235109822951472, -27.13685080543958250 ) ) ;
#4721 = VERTEX_POINT ( 'NONE', #9756 ) ;
#4722 = PLANE ( 'NONE',  #7056 ) ;
#4723 = DIRECTION ( 'NONE',  ( 0.000000000000000000, 0.000000000000000000, -1.000000000000000000 ) ) ;
#4724 = ORIENTED_EDGE ( 'NONE', *, *, #9813, .T. ) ;
#4725 = LINE ( 'NONE', #5426, #197 ) ;
#4726 = EDGE_CURVE ( 'NONE', #2418, #12307, #9880, .T. ) ;
#4727 = ORIENTED_EDGE ( 'NONE', *, *, #9593, .F. ) ;
#4728 = LINE ( 'NONE', #5858, #969 ) ;
#4729 = CARTESIAN_POINT ( 'NONE',  ( -30.00100000000000122, 85.26794919243110371, 9.660254037844429931 ) ) ;
#4730 = ORIENTED_EDGE ( 'NONE', *, *, #10868, .F. ) ;
#4731 = CARTESIAN_POINT ( 'NONE',  ( 0.000000000000000000, 290.0000000000000568, 0.000000000000000000 ) ) ;
#4732 = LINE ( 'NONE', #3802, #4905 ) ;
#4733 = ORIENTED_EDGE ( 'NONE', *, *, #1822, .T. ) ;
#4734 = ITEM_DEFINED_TRANSFORMATION ( 'NONE', 'NONE', #11932,  #1612 ) ;
#4735 = CARTESIAN_POINT ( 'NONE',  ( 11.80921887069467324, 29.75000000000018474, 80.00000000000000000 ) ) ;
#4736 = CARTESIAN_POINT ( 'NONE',  ( 3.250000000000000444, 114.4374999986344079, 0.000000000000000000 ) ) ;
#4737 = DIRECTION ( 'NONE',  ( -1.000000000000000000, 1.387778780781445676E-14, 0.000000000000000000 ) ) ;
#4738 = CIRCLE ( 'NONE', #5747, 3.399999999999999911 ) ;
#4739 = MECHANICAL_DESIGN_GEOMETRIC_PRESENTATION_REPRESENTATION (  '', ( #1985 ), #386 ) ;
#4740 = ORIENTED_EDGE ( 'NONE', *, *, #10703, .F. ) ;
#4741 = CARTESIAN_POINT ( 'NONE',  ( 2.708734124999999437, 111.4999999986343937, -1.121994411437820638 ) ) ;
#4742 = EDGE_CURVE ( 'NONE', #1244, #6757, #11267, .T. ) ;
#4743 = PRODUCT_DEFINITION ( 'UNKNOWN', '', #1969, #9497 ) ;
#4744 = EDGE_CURVE ( 'NONE', #4364, #7558, #3281, .T. ) ;
#4745 = CARTESIAN_POINT ( 'NONE',  ( 3.250000000000000444, 111.8749999972688158, 0.000000000000000000 ) ) ;
#4746 = ORIENTED_EDGE ( 'NONE', *, *, #8736, .F. ) ;
#4747 = AXIS2_PLACEMENT_3D ( 'NONE', #4581, #911, #1658 ) ;
#4748 = CARTESIAN_POINT ( 'NONE',  ( 0.000000000000000000, 87.50000000000000000, 0.000000000000000000 ) ) ;
#4749 = COLOUR_RGB ( '', 0.66274510, 0.83137255, 0.94901961) ;
#4750 = CARTESIAN_POINT ( 'NONE',  ( 69.72092797052471269, 43.18961593336220517, 27.64057077031492327 ) ) ;
#4751 = ORIENTED_EDGE ( 'NONE', *, *, #2050, .T. ) ;
#4752 = DIRECTION ( 'NONE',  ( 0.000000000000000000, 0.000000000000000000, 1.000000000000000000 ) ) ;
#4753 = CYLINDRICAL_SURFACE ( 'NONE', #3903, 30.00000000000000711 ) ;
#4754 = ORIENTED_EDGE ( 'NONE', *, *, #6785, .T. ) ;
#4755 = CARTESIAN_POINT ( 'NONE',  ( 30.00100000000000122, 85.26794919243110371, -9.660254037844429931 ) ) ;
#4756 = CARTESIAN_POINT ( 'NONE',  ( -14.19078112930533209, 29.75000000000008882, 79.50000000000000000 ) ) ;
#4757 = DIRECTION ( 'NONE',  ( 0.000000000000000000, 0.000000000000000000, -1.000000000000000000 ) ) ;
#4758 = EDGE_CURVE ( 'NONE', #4939, #8296, #9844, .T. ) ;
#4759 = CARTESIAN_POINT ( 'NONE',  ( -2.708734124999999882, 113.9999999986344079, 1.121994411437819084 ) ) ;
#4760 = ORIENTED_EDGE ( 'NONE', *, *, #7217, .T. ) ;
#4761 = ORIENTED_EDGE ( 'NONE', *, *, #1240, .T. ) ;
#4762 = DIRECTION ( 'NONE',  ( 1.000000000000000000, 0.000000000000000000, 0.000000000000000000 ) ) ;
#4763 = DIRECTION ( 'NONE',  ( 1.000000000000000000, 0.000000000000000000, 0.000000000000000000 ) ) ;
#4764 = EDGE_LOOP ( 'NONE', ( #4667, #10401, #3145, #375 ) ) ;
#4765 = CARTESIAN_POINT ( 'NONE',  ( -13.00000000000000178, 127.0000000000000000, -7.483314773547880883 ) ) ;
#4766 = CIRCLE ( 'NONE', #7759, 105.0000000000000426 ) ;
#4767 = CIRCLE ( 'NONE', #11743, 9.999999999999994671 ) ;
#4768 = DIRECTION ( 'NONE',  ( -0.000000000000000000, -1.000000000000000000, -0.000000000000000000 ) ) ;
#4769 =( NAMED_UNIT ( * ) PLANE_ANGLE_UNIT ( ) SI_UNIT ( $, .RADIAN. ) );
#4770 = DIRECTION ( 'NONE',  ( 0.000000000000000000, 1.000000000000000000, 0.000000000000000000 ) ) ;
#4771 = EDGE_CURVE ( 'NONE', #3440, #2446, #6284, .T. ) ;
#4772 = VECTOR ( 'NONE', #11405, 1000.000000000000114 ) ;
#4773 = EDGE_CURVE ( 'NONE', #3622, #4939, #4279, .T. ) ;
#4774 = CIRCLE ( 'NONE', #2185, 2.055000000000000160 ) ;
#4775 = UNCERTAINTY_MEASURE_WITH_UNIT (LENGTH_MEASURE( 1.000000000000000082E-05 ), #10936, 'distance_accuracy_value', 'NONE');
#4776 = CARTESIAN_POINT ( 'NONE',  ( 70.93011667421792765, 42.07610065776023589, -24.58871393576316677 ) ) ;
#4777 =( NAMED_UNIT ( * ) PLANE_ANGLE_UNIT ( ) SI_UNIT ( $, .RADIAN. ) );
#4778 = ORIENTED_EDGE ( 'NONE', *, *, #2732, .T. ) ;
#4779 = CARTESIAN_POINT ( 'NONE',  ( 31.65330186654243505, 85.26794919243108950, 9.660254037844429931 ) ) ;
#4780 = DIRECTION ( 'NONE',  ( 0.000000000000000000, 1.000000000000000000, -1.287488025362403787E-15 ) ) ;
#4781 = LINE ( 'NONE', #5787, #8457 ) ;
#4782 = CARTESIAN_POINT ( 'NONE',  ( 71.78382695943247427, 10.51293989489658642, -21.72958296927679456 ) ) ;
#4783 = ORIENTED_EDGE ( 'NONE', *, *, #19, .F. ) ;
#4784 = VECTOR ( 'NONE', #3539, 1000.000000000000227 ) ;
#4785 = CARTESIAN_POINT ( 'NONE',  ( 0.000000000000000000, 115.0000000000000000, 3.250000000000000444 ) ) ;
#4786 = CARTESIAN_POINT ( 'NONE',  ( 2.979367062500000163, 114.7187499979516190, 0.000000000000000000 ) ) ;
#4787 = EDGE_LOOP ( 'NONE', ( #10335, #6411, #4663, #10434 ) ) ;
#4788 = DIRECTION ( 'NONE',  ( 0.000000000000000000, -1.000000000000000000, 0.000000000000000000 ) ) ;
#4789 = ADVANCED_FACE ( 'NONE', ( #228 ), #7538, .F. ) ;
#4790 = AXIS2_PLACEMENT_3D ( 'NONE', #6816, #1084, #4073 ) ;
#4791 = VECTOR ( 'NONE', #11391, 1000.000000000000000 ) ;
#4792 = B_SPLINE_CURVE_WITH_KNOTS ( 'NONE', 3,
 ( #4411, #4474, #3482, #1552 ),
 .UNSPECIFIED., .F., .F.,
 ( 4, 4 ),
 ( 0.0002502309401078514238, 0.0005002309401076744872 ),
 .UNSPECIFIED. ) ;
#4793 = EDGE_CURVE ( 'NONE', #3205, #6749, #11243, .T. ) ;
#4794 = ORIENTED_EDGE ( 'NONE', *, *, #5822, .T. ) ;
#4795 = CARTESIAN_POINT ( 'NONE',  ( 25.00000000000000355, 445.0000000000000568, -90.00000000000000000 ) ) ;
#4796 = CARTESIAN_POINT ( 'NONE',  ( -1.190781129305471087, 30.00000000000008882, 78.00000000000000000 ) ) ;
#4797 = ORIENTED_EDGE ( 'NONE', *, *, #4953, .T. ) ;
#4798 = CARTESIAN_POINT ( 'NONE',  ( 33.64113847583112715, 77.00000000000000000, -8.529771698700599813 ) ) ;
#4799 = CARTESIAN_POINT ( 'NONE',  ( -20.00000000000000000, 7.965803112215716020, -67.08203932499371547 ) ) ;
#4800 = ORIENTED_EDGE ( 'NONE', *, *, #12134, .T. ) ;
#4801 = APPLICATION_PROTOCOL_DEFINITION ( 'draft international standard', 'automotive_design', 1998, #2548 ) ;
#4802 = FACE_BOUND ( 'NONE', #6451, .T. ) ;
#4804 = CARTESIAN_POINT ( 'NONE',  ( -5.974274778359173865, 21.21474596215567487, 79.50000000000000000 ) ) ;
#4803 = AXIS2_PLACEMENT_3D ( 'NONE', #827, #4618, #1698 ) ;
#4805 = DIRECTION ( 'NONE',  ( 0.000000000000000000, 0.000000000000000000, -1.000000000000000000 ) ) ;
#4806 = EDGE_CURVE ( 'NONE', #8730, #893, #10006, .T. ) ;
#4807 = EDGE_CURVE ( 'NONE', #5440, #11360, #663, .T. ) ;
#4808 = VERTEX_POINT ( 'NONE', #2402 ) ;
#4809 = CARTESIAN_POINT ( 'NONE',  ( -1.121994411437818862, 113.8749999986343937, 2.708734124999999882 ) ) ;
#4810 = CARTESIAN_POINT ( 'NONE',  ( 3.250000000000000444, 110.9374999972688016, 1.346194077712559389 ) ) ;
#4811 = CIRCLE ( 'NONE', #5414, 15.00000000000000000 ) ;
#4812 = AXIS2_PLACEMENT_3D ( 'NONE', #8133, #10189, #2474 ) ;
#4813 = EDGE_LOOP ( 'NONE', ( #8218, #4, #2570, #6223 ) ) ;
#4814 = DIRECTION ( 'NONE',  ( 0.000000000000000000, 0.000000000000000000, -1.000000000000000000 ) ) ;
#4815 = CARTESIAN_POINT ( 'NONE',  ( -9.797345851249669835, 17.67135281155243476, 74.36268359007875972 ) ) ;
#4816 = ORIENTED_EDGE ( 'NONE', *, *, #1063, .F. ) ;
#4817 = CARTESIAN_POINT ( 'NONE',  ( -30.00100000000000122, 77.00000000000000000, -4.660254037844413944 ) ) ;
#4818 = CARTESIAN_POINT ( 'NONE',  ( 70.26526821373037990, 13.93439898317257430, 26.22825182065056637 ) ) ;
#4819 = VERTEX_POINT ( 'NONE', #2472 ) ;
#4820 = PRODUCT_RELATED_PRODUCT_CATEGORY ( 'part', '', ( #8763 ) ) ;
#4821 = CARTESIAN_POINT ( 'NONE',  ( -20.00000000000000355, 50.00000000000000000, -57.08203932499370836 ) ) ;
#4822 = DIRECTION ( 'NONE',  ( 0.000000000000000000, 1.000000000000000000, 0.000000000000000000 ) ) ;
#4823 = DIRECTION ( 'NONE',  ( 1.000000000000000000, -1.040834085586083310E-14, 0.000000000000000000 ) ) ;
#4824 = CARTESIAN_POINT ( 'NONE',  ( 0.000000000000000000, 290.0000000000000568, -115.0000000000000284 ) ) ;
#4825 = DIRECTION ( 'NONE',  ( 0.000000000000000000, 0.000000000000000000, 1.000000000000000000 ) ) ;
#4826 = CARTESIAN_POINT ( 'NONE',  ( 1.121994411437819084, 112.7499999986344079, 2.708734124999999882 ) ) ;
#4827 = VERTEX_POINT ( 'NONE', #3590 ) ;
#4828 = VERTEX_POINT ( 'NONE', #8316 ) ;
#4829 = DIRECTION ( 'NONE',  ( 0.000000000000000000, -1.000000000000000000, 0.000000000000000000 ) ) ;
#4830 = EDGE_CURVE ( 'NONE', #6973, #1372, #6461, .T. ) ;
#4831 = CARTESIAN_POINT ( 'NONE',  ( 5.092712519748452848, 41.38333024919784719, 79.50000000000000000 ) ) ;
#4832 = AXIS2_PLACEMENT_3D ( 'NONE', #7575, #9492, #8561 ) ;
#4833 = VERTEX_POINT ( 'NONE', #11135 ) ;
#4834 = FACE_OUTER_BOUND ( 'NONE', #387, .T. ) ;
#4835 = DIRECTION ( 'NONE',  ( 0.000000000000000000, 0.000000000000000000, 1.000000000000000000 ) ) ;
#4836 = LINE ( 'NONE', #1967, #10072 ) ;
#4837 = PLANE ( 'NONE',  #1018 ) ;
#4838 = EDGE_CURVE ( 'NONE', #10836, #11371, #6215, .T. ) ;
#4839 = VERTEX_POINT ( 'NONE', #7399 ) ;
#4840 =( NAMED_UNIT ( * ) PLANE_ANGLE_UNIT ( ) SI_UNIT ( $, .RADIAN. ) );
#4841 = ORIENTED_EDGE ( 'NONE', *, *, #5560, .F. ) ;
#4842 = VECTOR ( 'NONE', #8282, 1000.000000000000000 ) ;
#4843 = CARTESIAN_POINT ( 'NONE',  ( 71.40110041869772317, 44.02658904323298117, -23.12535642331799579 ) ) ;
#4844 =( NAMED_UNIT ( * ) SI_UNIT ( $, .STERADIAN. ) SOLID_ANGLE_UNIT ( ) );
#4845 = ADVANCED_FACE ( 'NONE', ( #3533 ), #2592, .F. ) ;
#4846 = DIRECTION ( 'NONE',  ( 0.000000000000000000, 0.000000000000000000, -1.000000000000000000 ) ) ;
#4847 = DIRECTION ( 'NONE',  ( 0.000000000000000000, 0.000000000000000000, -1.000000000000000000 ) ) ;
#4848 = DIRECTION ( 'NONE',  ( -0.4999999999999933387, 0.8660254037844424824, 0.000000000000000000 ) ) ;
#4849 = CARTESIAN_POINT ( 'NONE',  ( 71.89872685388522200, 15.05565339638229716, -21.44363277848739457 ) ) ;
#4850 = ORIENTED_EDGE ( 'NONE', *, *, #5364, .F. ) ;
#4851 = VECTOR ( 'NONE', #3094, 1000.000000000000114 ) ;
#4852 = CARTESIAN_POINT ( 'NONE',  ( -32.05000697088088657, 85.26794919243110371, -9.660254037844429931 ) ) ;
#4853 = CARTESIAN_POINT ( 'NONE',  ( 2.500000000000000000, 2.357898499370431722, -2.818925648462311528E-15 ) ) ;
#4854 = ORIENTED_EDGE ( 'NONE', *, *, #5726, .T. ) ;
#4855 = CARTESIAN_POINT ( 'NONE',  ( 0.000000000000000000, 92.00000000000000000, 0.000000000000000000 ) ) ;
#4856 = AXIS2_PLACEMENT_3D ( 'NONE', #10498, #4829, #4642 ) ;
#4857 = VECTOR ( 'NONE', #7368, 1000.000000000000000 ) ;
#4858 = ORIENTED_EDGE ( 'NONE', *, *, #1845, .F. ) ;
#4859 = CARTESIAN_POINT ( 'NONE',  ( 6.000000000000000000, 50.00000000000000000, 70.00000000000001421 ) ) ;
#4860 = CARTESIAN_POINT ( 'NONE',  ( 20.00000000000000355, 7.965803112215716020, 57.08203932499370836 ) ) ;
#4861 = VERTEX_POINT ( 'NONE', #6399 ) ;
#4862 = APPLICATION_CONTEXT ( 'automotive_design' ) ;
#4863 = DIRECTION ( 'NONE',  ( 1.000000000000000000, 0.000000000000000000, 0.000000000000000000 ) ) ;
#4864 = CARTESIAN_POINT ( 'NONE',  ( 10.19254911989241386, 23.71650635094626836, 79.50000000000000000 ) ) ;
#4865 = ORIENTED_EDGE ( 'NONE', *, *, #9903, .F. ) ;
#4866 = ADVANCED_FACE ( 'NONE', ( #5283 ), #9271, .F. ) ;
#4867 = APPLICATION_PROTOCOL_DEFINITION ( 'draft international standard', 'automotive_design', 1998, #397 ) ;
#4868 = DIRECTION ( 'NONE',  ( -0.000000000000000000, -1.000000000000000000, -0.000000000000000000 ) ) ;
#4869 = DIRECTION ( 'NONE',  ( -0.000000000000000000, -1.000000000000000000, -0.000000000000000000 ) ) ;
#4870 = LINE ( 'NONE', #8658, #7791 ) ;
#4871 = TOROIDAL_SURFACE ( 'NONE', #1682, 80.00000000000001421, 5.000000000000000000 ) ;
#4872 = ORIENTED_EDGE ( 'NONE', *, *, #4577, .T. ) ;
#4873 = CARTESIAN_POINT ( 'NONE',  ( -1.121994411437818862, 112.6249999986343937, 2.708734125000000326 ) ) ;
#4874 = AXIS2_PLACEMENT_3D ( 'NONE', #9201, #3486, #8274 ) ;
#4875 = CARTESIAN_POINT ( 'NONE',  ( -0.9407811293052825707, 17.00000000000008882, 79.50000000000000000 ) ) ;
#4876 = ORIENTED_EDGE ( 'NONE', *, *, #7108, .T. ) ;
#4877 = EDGE_CURVE ( 'NONE', #11869, #10169, #4683, .T. ) ;
#4878 = DIRECTION ( 'NONE',  ( -1.000000000000000000, 0.000000000000000000, -0.000000000000000000 ) ) ;
#4879 = EDGE_CURVE ( 'NONE', #7492, #9390, #3410, .T. ) ;
#4880 = CARTESIAN_POINT ( 'NONE',  ( -8.467961960366615415, 16.87331863704340762, 74.52176054247227910 ) ) ;
#4881 = CIRCLE ( 'NONE', #493, 105.0000000000000426 ) ;
#4882 = EDGE_LOOP ( 'NONE', ( #6264, #10031, #6481, #5008 ) ) ;
#4883 = AXIS2_PLACEMENT_3D ( 'NONE', #10604, #4001, #10971 ) ;
#4884 = DIRECTION ( 'NONE',  ( 7.011174048739587977E-15, 1.000000000000000000, 0.000000000000000000 ) ) ;
#4885 = CARTESIAN_POINT ( 'NONE',  ( -24.99999999999999645, 445.0000000000000568, -105.0000000000000000 ) ) ;
#4886 = ORIENTED_EDGE ( 'NONE', *, *, #3334, .T. ) ;
#4887 = CARTESIAN_POINT ( 'NONE',  ( 7.344472908539098732, 24.78349364905406205, 79.50000000000000000 ) ) ;
#4888 = CARTESIAN_POINT ( 'NONE',  ( 32.15778161310143446, 87.00000000000000000, 8.660254037844435260 ) ) ;
#4889 = FACE_OUTER_BOUND ( 'NONE', #8531, .T. ) ;
#4890 = CARTESIAN_POINT ( 'NONE',  ( 72.04250006633355952, 10.25027406420806031, 20.85600298363943494 ) ) ;
#4891 = VECTOR ( 'NONE', #10730, 1000.000000000000000 ) ;
#4892 = ORIENTED_EDGE ( 'NONE', *, *, #7315, .F. ) ;
#4893 =( NAMED_UNIT ( * ) PLANE_ANGLE_UNIT ( ) SI_UNIT ( $, .RADIAN. ) );
#4894 = VECTOR ( 'NONE', #1447, 1000.000000000000000 ) ;
#4895 = VERTEX_POINT ( 'NONE', #1726 ) ;
#4896 = FACE_OUTER_BOUND ( 'NONE', #1156, .T. ) ;
#4897 = CARTESIAN_POINT ( 'NONE',  ( 13.80921887069452758, 30.00000000000009237, 73.71774192269630532 ) ) ;
#4898 = VERTEX_POINT ( 'NONE', #2651 ) ;
#4899 = DIRECTION ( 'NONE',  ( 0.000000000000000000, 1.000000000000000000, 0.000000000000000000 ) ) ;
#4900 = AXIS2_PLACEMENT_3D ( 'NONE', #838, #11183, #4630 ) ;
#4901 = CARTESIAN_POINT ( 'NONE',  ( 0.000000000000000000, 63.00000000000000000, -57.08203932499371547 ) ) ;
#4902 = SURFACE_STYLE_USAGE ( .BOTH. , #3905 ) ;
#4903 = CARTESIAN_POINT ( 'NONE',  ( 0.000000000000000000, 92.00000000000000000, 0.000000000000000000 ) ) ;
#4904 = ORIENTED_EDGE ( 'NONE', *, *, #6203, .T. ) ;
#4905 = VECTOR ( 'NONE', #2864, 1000.000000000000114 ) ;
#4906 = VERTEX_POINT ( 'NONE', #8378 ) ;
#4907 = EDGE_CURVE ( 'NONE', #1153, #5440, #2715, .T. ) ;
#4908 = ORIENTED_EDGE ( 'NONE', *, *, #6422, .F. ) ;
#4909 = ADVANCED_FACE ( 'NONE', ( #9666 ), #8850, .T. ) ;
#4910 = EDGE_CURVE ( 'NONE', #2329, #2522, #2193, .T. ) ;
#4911 = CARTESIAN_POINT ( 'NONE',  ( 71.54629459846562156, 44.36298584812474388, -22.64784456521648437 ) ) ;
#4912 = VECTOR ( 'NONE', #2652, 1000.000000000000000 ) ;
#4913 = SURFACE_SIDE_STYLE ('',( #32 ) ) ;
#4914 = CARTESIAN_POINT ( 'NONE',  ( 30.12465603153684413, 85.44772375131799436, 9.971632707744760182 ) ) ;
#4915 = DIRECTION ( 'NONE',  ( 0.000000000000000000, 0.000000000000000000, 1.000000000000000000 ) ) ;
#4916 = PLANE ( 'NONE',  #5476 ) ;
#4917 = CARTESIAN_POINT ( 'NONE',  ( 71.40290628601607636, 15.98094810295091861, -23.11746242201430945 ) ) ;
#4918 = VERTEX_POINT ( 'NONE', #2138 ) ;
#4919 = CARTESIAN_POINT ( 'NONE',  ( 5.092712519748611832, 18.61666975080242992, 79.50000000000000000 ) ) ;
#4920 = DIRECTION ( 'NONE',  ( 0.000000000000000000, 0.000000000000000000, -1.000000000000000000 ) ) ;
#4921 = ORIENTED_EDGE ( 'NONE', *, *, #548, .T. ) ;
#4922 = DIRECTION ( 'NONE',  ( -0.8660254037844385966, 0.5000000000000000000, 0.000000000000000000 ) ) ;
#4923 = VECTOR ( 'NONE', #5391, 1000.000000000000000 ) ;
#4924 = ORIENTED_EDGE ( 'NONE', *, *, #11098, .F. ) ;
#4925 = DIRECTION ( 'NONE',  ( 1.000000000000000000, 0.000000000000000000, 0.000000000000000000 ) ) ;
#4926 = CARTESIAN_POINT ( 'NONE',  ( 76.77294714683046095, 44.85115178501149558, 21.25082451143517304 ) ) ;
#4927 = ORIENTED_EDGE ( 'NONE', *, *, #9330, .T. ) ;
#4928 = DIRECTION ( 'NONE',  ( 0.000000000000000000, 1.000000000000000000, 0.000000000000000000 ) ) ;
#4929 = DIRECTION ( 'NONE',  ( 0.000000000000000000, 1.000000000000000000, 0.000000000000000000 ) ) ;
#4930 = ORIENTED_EDGE ( 'NONE', *, *, #7084, .T. ) ;
#4931 = SHAPE_DEFINITION_REPRESENTATION ( #5691, #8876 ) ;
#4932 = CARTESIAN_POINT ( 'NONE',  ( 150.0000000000011084, 15.00000000000011724, 20.00000000000000000 ) ) ;
#4933 = CARTESIAN_POINT ( 'NONE',  ( 100.7495955565343451, 275.0000000000000000, 29.57226733266770680 ) ) ;
#4934 = ORIENTED_EDGE ( 'NONE', *, *, #7052, .F. ) ;
#4935 = CARTESIAN_POINT ( 'NONE',  ( -4.975863863883684959E-16, 113.0624999986344079, -2.708734125000000326 ) ) ;
#4936 = CARTESIAN_POINT ( 'NONE',  ( 2.298097038856278918, 112.7499999972688158, -2.298097038856279806 ) ) ;
#4937 = ADVANCED_FACE ( 'NONE', ( #5941, #6750 ), #1082, .T. ) ;
#4938 = EDGE_CURVE ( 'NONE', #4906, #4833, #11499, .T. ) ;
#4939 = VERTEX_POINT ( 'NONE', #7861 ) ;
#4940 = PLANE ( 'NONE',  #588 ) ;
#4941 = DIRECTION ( 'NONE',  ( 0.000000000000000000, 1.000000000000000000, 0.000000000000000000 ) ) ;
#4942 = ORIENTED_EDGE ( 'NONE', *, *, #11765, .F. ) ;
#4943 = CARTESIAN_POINT ( 'NONE',  ( -9.726035167149685634, 24.78349364905394125, 79.50000000000000000 ) ) ;
#4944 = FACE_OUTER_BOUND ( 'NONE', #10202, .T. ) ;
#4945 = AXIS2_PLACEMENT_3D ( 'NONE', #8337, #560, #7300 ) ;
#4946 = ORIENTED_EDGE ( 'NONE', *, *, #996, .F. ) ;
#4947 = CARTESIAN_POINT ( 'NONE',  ( -3.250000000000000444, 110.4375000000000000, 1.346194077712559167 ) ) ;
#4948 = DIRECTION ( 'NONE',  ( 1.049727191138619928E-16, 0.5150380749100523792, -0.8571673007021134438 ) ) ;
#4949 = CARTESIAN_POINT ( 'NONE',  ( 0.000000000000000000, 65.00000000000000000, 0.000000000000000000 ) ) ;
#4950 = CARTESIAN_POINT ( 'NONE',  ( -11.19078112930532853, 29.75000000000005684, 80.00000000000000000 ) ) ;
#4951 = DIRECTION ( 'NONE',  ( -1.000000000000000000, 0.000000000000000000, -0.000000000000000000 ) ) ;
#4952 = CARTESIAN_POINT ( 'NONE',  ( 1.121994411437819084, 113.3749999986344079, -2.708734124999999437 ) ) ;
#4953 = EDGE_CURVE ( 'NONE', #7931, #9228, #6683, .T. ) ;
#4954 = AXIS2_PLACEMENT_3D ( 'NONE', #660, #8772, #5337 ) ;
#4955 = EDGE_CURVE ( 'NONE', #7513, #11122, #7683, .T. ) ;
#4956 = ORIENTED_EDGE ( 'NONE', *, *, #6848, .F. ) ;
#4957 = DIRECTION ( 'NONE',  ( 0.000000000000000000, 1.000000000000000000, 0.000000000000000000 ) ) ;
#4958 = CARTESIAN_POINT ( 'NONE',  ( 11.76642283301164937, 37.57159100124651729, 74.07168364809568573 ) ) ;
#4959 = ORIENTED_EDGE ( 'NONE', *, *, #3344, .T. ) ;
#4960 = FACE_OUTER_BOUND ( 'NONE', #4991, .T. ) ;
#4961 = CARTESIAN_POINT ( 'NONE',  ( -109.9268209223825750, 285.0000000000000568, 32.26598893414599445 ) ) ;
#4962 = FILL_AREA_STYLE_COLOUR ( '', #118 ) ;
#4963 = CARTESIAN_POINT ( 'NONE',  ( 2.708734125000000326, 111.3749999986344079, 1.121994411437819084 ) ) ;
#4964 = ADVANCED_FACE ( 'NONE', ( #29 ), #413, .T. ) ;
#4965 = VERTEX_POINT ( 'NONE', #2949 ) ;
#4966 = ADVANCED_FACE ( 'NONE', ( #2076 ), #1203, .F. ) ;
#4967 = ADVANCED_FACE ( 'NONE', ( #9789 ), #6936, .T. ) ;
#4968 = ORIENTED_EDGE ( 'NONE', *, *, #12131, .F. ) ;
#4969 = AXIS2_PLACEMENT_3D ( 'NONE', #5281, #10186, #9061 ) ;
#4970 = CARTESIAN_POINT ( 'NONE',  ( 0.000000000000000000, 265.0000000000000000, -98.00000000000001421 ) ) ;
#4971 = CARTESIAN_POINT ( 'NONE',  ( 8.809218870694669690, 29.75000000000019540, 80.00000000000000000 ) ) ;
#4972 = DIRECTION ( 'NONE',  ( 7.011174048739587977E-15, 1.000000000000000000, 0.000000000000000000 ) ) ;
#4973 = LINE ( 'NONE', #7146, #9856 ) ;
#4974 = CARTESIAN_POINT ( 'NONE',  ( 76.47662455941971871, 15.31021820271415024, -21.74119912862034454 ) ) ;
#4975 = EDGE_LOOP ( 'NONE', ( #1950, #1002, #3909, #9130 ) ) ;
#4976 = PRODUCT_RELATED_PRODUCT_CATEGORY ( 'part', '', ( #8455 ) ) ;
#4977 = FACE_OUTER_BOUND ( 'NONE', #5687, .T. ) ;
#4978 = EDGE_CURVE ( 'NONE', #1236, #1442, #193, .T. ) ;
#4979 = CARTESIAN_POINT ( 'NONE',  ( 0.000000000000000000, 260.0000000000000000, 105.0000000000000426 ) ) ;
#4980 = AXIS2_PLACEMENT_3D ( 'NONE', #4478, #11153, #11651 ) ;
#4981 = ORIENTED_EDGE ( 'NONE', *, *, #4419, .T. ) ;
#4982 = DIRECTION ( 'NONE',  ( -0.000000000000000000, 1.000000000000000000, -0.000000000000000000 ) ) ;
#4983 = ORIENTED_EDGE ( 'NONE', *, *, #2199, .T. ) ;
#4984 = DIRECTION ( 'NONE',  ( -0.000000000000000000, -1.000000000000000000, -0.000000000000000000 ) ) ;
#4985 = AXIS2_PLACEMENT_3D ( 'NONE', #1437, #11097, #5303 ) ;
#4986 = CARTESIAN_POINT ( 'NONE',  ( 74.62285592809365653, 42.36573936498655257, 24.41804092124679215 ) ) ;
#4987 = ORIENTED_EDGE ( 'NONE', *, *, #10117, .F. ) ;
#4988 = CARTESIAN_POINT ( 'NONE',  ( 32.15133482848810331, 77.00000000000000000, -7.827692000169491848 ) ) ;
#4989 = EDGE_CURVE ( 'NONE', #3450, #5494, #6643, .T. ) ;
#4990 = DIRECTION ( 'NONE',  ( -1.000000000000000000, -0.000000000000000000, -0.000000000000000000 ) ) ;
#4991 = EDGE_LOOP ( 'NONE', ( #11788, #11618, #11193, #2044 ) ) ;
#4992 = DIRECTION ( 'NONE',  ( 0.000000000000000000, 0.000000000000000000, -1.000000000000000000 ) ) ;
#4993 = DIRECTION ( 'NONE',  ( 1.000000000000000000, 0.000000000000000000, 0.000000000000000000 ) ) ;
#4994 = ORIENTED_EDGE ( 'NONE', *, *, #2158, .F. ) ;
#4995 = CARTESIAN_POINT ( 'NONE',  ( 1.121994411437819528, 113.1249999986343937, -2.708734124999999882 ) ) ;
#4996 = CARTESIAN_POINT ( 'NONE',  ( -3.250000000000001776, 111.4374999972688300, -1.346194077712558723 ) ) ;
#4997 = AXIS2_PLACEMENT_3D ( 'NONE', #2229, #6101, #9885 ) ;
#4998 = VECTOR ( 'NONE', #2902, 1000.000000000000000 ) ;
#4999 = ORIENTED_EDGE ( 'NONE', *, *, #153, .F. ) ;
#5000 = DIRECTION ( 'NONE',  ( 0.000000000000000000, -0.000000000000000000, 1.000000000000000000 ) ) ;
#5001 = CARTESIAN_POINT ( 'NONE',  ( -1.040515751868670957, 14.96447674105763070, 75.00000000000001421 ) ) ;
#5002 = ORIENTED_EDGE ( 'NONE', *, *, #11083, .T. ) ;
#5003 = FACE_OUTER_BOUND ( 'NONE', #2865, .T. ) ;
#5004 = DIRECTION ( 'NONE',  ( 0.2499999999999996669, 0.000000000000000000, -0.9682458365518542553 ) ) ;
#5005 = CIRCLE ( 'NONE', #3411, 5.000000000000000888 ) ;
#5006 = AXIS2_PLACEMENT_3D ( 'NONE', #5629, #8416, #12240 ) ;
#5007 = EDGE_CURVE ( 'NONE', #9831, #9708, #6527, .T. ) ;
#5008 = ORIENTED_EDGE ( 'NONE', *, *, #3560, .T. ) ;
#5009 = DIRECTION ( 'NONE',  ( 0.000000000000000000, 1.000000000000000000, 0.000000000000000000 ) ) ;
#5010 = DIRECTION ( 'NONE',  ( 0.000000000000000000, 0.000000000000000000, -1.000000000000000000 ) ) ;
#5011 = ADVANCED_FACE ( 'NONE', ( #259 ), #5075, .T. ) ;
#5012 = DIRECTION ( 'NONE',  ( 0.5000000000000036637, 0.8660254037844364872, 0.000000000000000000 ) ) ;
#5013 = DIRECTION ( 'NONE',  ( -1.000000000000000000, -0.000000000000000000, -0.000000000000000000 ) ) ;
#5014 = EDGE_CURVE ( 'NONE', #10740, #51, #9541, .T. ) ;
#5015 = AXIS2_PLACEMENT_3D ( 'NONE', #11985, #629, #2501 ) ;
#5016 = CARTESIAN_POINT ( 'NONE',  ( 2.708734124999999882, 112.5624999986344079, 0.000000000000000000 ) ) ;
#5017 = VECTOR ( 'NONE', #9064, 1000.000000000000000 ) ;
#5018 = EDGE_LOOP ( 'NONE', ( #5058, #4702, #4886, #497 ) ) ;
#5019 = ORIENTED_EDGE ( 'NONE', *, *, #6573, .T. ) ;
#5020 = CARTESIAN_POINT ( 'NONE',  ( 11.80921887069467324, 29.75000000000018474, 79.50000000000000000 ) ) ;
#5021 = CARTESIAN_POINT ( 'NONE',  ( 3.641433828188992639, 44.20809573012787297, 74.91284009398577837 ) ) ;
#5022 = VERTEX_POINT ( 'NONE', #70 ) ;
#5023 = CIRCLE ( 'NONE', #1831, 22.00000000000000355 ) ;
#5024 = DIRECTION ( 'NONE',  ( 0.8660254037844331565, -0.5000000000000095479, 0.000000000000000000 ) ) ;
#5025 = CARTESIAN_POINT ( 'NONE',  ( -1.346194077712548287, 112.5624999972688016, -3.250000000000012434 ) ) ;
#5026 = AXIS2_PLACEMENT_3D ( 'NONE', #11390, #2774, #12205 ) ;
#5027 =( NAMED_UNIT ( * ) SI_UNIT ( $, .STERADIAN. ) SOLID_ANGLE_UNIT ( ) );
#5028 = LINE ( 'NONE', #2212, #6787 ) ;
#5029 = ADVANCED_FACE ( 'NONE', ( #4244 ), #11866, .F. ) ;
#5030 = EDGE_CURVE ( 'NONE', #51, #9490, #2373, .T. ) ;
#5031 = ORIENTED_EDGE ( 'NONE', *, *, #7494, .F. ) ;
#5032 = DIRECTION ( 'NONE',  ( 1.000000000000000000, 0.000000000000000000, 0.000000000000000000 ) ) ;
#5033 = ORIENTED_EDGE ( 'NONE', *, *, #5221, .F. ) ;
#5034 = AXIS2_PLACEMENT_3D ( 'NONE', #7071, #10929, #5024 ) ;
#5035 =( NAMED_UNIT ( * ) SI_UNIT ( $, .STERADIAN. ) SOLID_ANGLE_UNIT ( ) );
#5036 = EDGE_CURVE ( 'NONE', #7852, #1429, #9912, .T. ) ;
#5037 = ADVANCED_FACE ( 'NONE', ( #8971 ), #10791, .F. ) ;
#5038 = DIRECTION ( 'NONE',  ( -0.000000000000000000, -1.000000000000000000, -0.000000000000000000 ) ) ;
#5039 = DIRECTION ( 'NONE',  ( 0.000000000000000000, 0.000000000000000000, 1.000000000000000000 ) ) ;
#5040 = CARTESIAN_POINT ( 'NONE',  ( 74.70253266892970601, 17.45276100714020728, -24.31510929947467048 ) ) ;
#5041 = CARTESIAN_POINT ( 'NONE',  ( 70.88057259133860555, 12.10784404089235800, -24.51542725512078391 ) ) ;
#5042 = CARTESIAN_POINT ( 'NONE',  ( 1.121994411437818862, 111.4999999986343937, 2.708734125000000326 ) ) ;
#5043 = AXIS2_PLACEMENT_3D ( 'NONE', #11295, #1686, #12226 ) ;
#5044 = ORIENTED_EDGE ( 'NONE', *, *, #8703, .F. ) ;
#5045 = CARTESIAN_POINT ( 'NONE',  ( -3.250000000000001776, 113.4374999972688300, -1.346194077712558279 ) ) ;
#5046 = ADVANCED_FACE ( 'NONE', ( #7176 ), #5093, .T. ) ;
#5047 =( BOUNDED_CURVE ( )  B_SPLINE_CURVE ( 2, ( #6260, #3518, #11120, #1395, #454, #4259, #9988, #7128, #1459 ),
 .UNSPECIFIED., .F., .F. ) 
 B_SPLINE_CURVE_WITH_KNOTS ( ( 3, 2, 2, 2, 3 ),
 ( 0.1875000000000001665, 0.2187500000000001943, 0.2500000000000002220, 0.2812500000000002220, 0.3125000000000002776 ),
 .UNSPECIFIED. ) 
 CURVE ( )  GEOMETRIC_REPRESENTATION_ITEM ( )  RATIONAL_B_SPLINE_CURVE ( ( 0.9999999999999995559, 0.9238795325112871826, 1.000000000000000000, 0.9238795325112867385, 1.000000000000000000, 0.9238795325112867385, 1.000000000000000000, 0.9238795325112860723, 1.000000000000000666 ) ) 
 REPRESENTATION_ITEM ( '' )  );
#5048 = PRODUCT_DEFINITION ( 'UNKNOWN', '', #2561, #7007 ) ;
#5049 = ORIENTED_EDGE ( 'NONE', *, *, #11667, .T. ) ;
#5050 = CONICAL_SURFACE ( 'NONE', #5453, 2.041999999999999815, 1.047197551196591858 ) ;
#5051 = DIRECTION ( 'NONE',  ( -0.2358520287683116834, 0.000000000000000000, 0.9717889794219068955 ) ) ;
#5052 = VERTEX_POINT ( 'NONE', #6246 ) ;
#5053 = DIRECTION ( 'NONE',  ( -0.000000000000000000, 1.000000000000000000, -0.000000000000000000 ) ) ;
#5054 = CARTESIAN_POINT ( 'NONE',  ( 27.95322648060798087, 86.18856968700900723, 11.45194355884130388 ) ) ;
#5055 = ORIENTED_EDGE ( 'NONE', *, *, #4637, .T. ) ;
#5056 = DIRECTION ( 'NONE',  ( -1.000000000000000000, 0.000000000000000000, 0.000000000000000000 ) ) ;
#5057 = PLANE ( 'NONE',  #16 ) ;
#5058 = ORIENTED_EDGE ( 'NONE', *, *, #2766, .F. ) ;
#5059 = CARTESIAN_POINT ( 'NONE',  ( -1.915364268218909816, 110.9374999986344079, -1.915364268218909150 ) ) ;
#5060 = AXIS2_PLACEMENT_3D ( 'NONE', #11769, #1289, #8938 ) ;
#5061 = CARTESIAN_POINT ( 'NONE',  ( 3.250000000000000444, 113.8749999972688158, 0.000000000000000000 ) ) ;
#5062 = AXIS2_PLACEMENT_3D ( 'NONE', #2467, #593, #8251 ) ;
#5063 = ADVANCED_FACE ( 'NONE', ( #10036 ), #7977, .F. ) ;
#5064 = EDGE_CURVE ( 'NONE', #12107, #4302, #7918, .T. ) ;
#5065 = ORIENTED_EDGE ( 'NONE', *, *, #11848, .F. ) ;
#5066 = CARTESIAN_POINT ( 'NONE',  ( 0.000000000000000000, 10.00000000000017586, -75.00000000000001421 ) ) ;
#5067 = ADVANCED_FACE ( 'NONE', ( #568 ), #6993, .F. ) ;
#5068 = CARTESIAN_POINT ( 'NONE',  ( 145.0000000000011369, 230.0000000000000853, 25.00000000000000000 ) ) ;
#5069 = ORIENTED_EDGE ( 'NONE', *, *, #10117, .T. ) ;
#5070 = PLANE ( 'NONE',  #11581 ) ;
#5071 = FACE_OUTER_BOUND ( 'NONE', #2984, .T. ) ;
#5072 = ORIENTED_EDGE ( 'NONE', *, *, #9997, .F. ) ;
#5073 = VECTOR ( 'NONE', #959, 1000.000000000000114 ) ;
#5074 =( BOUNDED_SURFACE ( )  B_SPLINE_SURFACE ( 1, 2, ( 
 ( #6659, #232, #10700, #103, #167, #3977, #5732, #7654, #1115, #10947, #2346, #289, #2408, #7092, #11838, #4099, #9066, #10010, #7890, #5042, #7150, #11012, #1295, #1355, #9943, #5106, #8823, #4283, #11709, #10889, #8077, #4221, #3416, #1235, #6098, #4338, #3161, #6219, #5164, #8012, #11901, #7025, #3287, #5289, #2227, #8943, #6964, #1481, #9821, #6034, #6153, #10767, #2478, #3228, #1419, #3353, #416, #9883, #5227, #9003, #478, #540, #8886, #350, #7213 ),
 ( #8135, #11956, #11778, #6278, #10825, #4156, #7948, #2288, #11437, #8383, #10492, #10256, #4531, #2954, #8615, #4466, #4588, #3593, #7405, #2598, #12019, #10192, #11503, #8196, #74, #1730, #1604, #10069, #12087, #2539, #9254, #11139, #8262, #10127, #796, #7341, #5766, #7688, #1544, #5412, #5536, #2654, #13, #9189, #668, #1664, #9546, #3891, #738, #3475, #6341, #605, #2887, #6696, #5347, #3538, #6405, #1026, #9315, #8321, #12144, #5473, #1954, #11205, #4401 ) ),
 .UNSPECIFIED., .F., .F., .T. ) 
 B_SPLINE_SURFACE_WITH_KNOTS ( ( 2, 2 ),
 ( 3, 2, 2, 2, 2, 2, 2, 2, 2, 2, 2, 2, 2, 2, 2, 2, 2, 2, 2, 2, 2, 2, 2, 2, 2, 2, 2, 2, 2, 2, 2, 2, 3 ),
 ( 0.000000000000000000, 1.000000000000000000 ),
 ( 0.000000000000000000, 0.03125000000000000000, 0.06250000000000000000, 0.09375000000000000000, 0.1250000000000000000, 0.1562500000000000000, 0.1875000000000000000, 0.2187500000000000000, 0.2500000000000000000, 0.2812500000000000000, 0.3125000000000000000, 0.3437500000000000000, 0.3750000000000000000, 0.4062500000000000000, 0.4375000000000000000, 0.4687500000000000000, 0.5000000000000000000, 0.5312500000000000000, 0.5625000000000000000, 0.5937500000000000000, 0.6250000000000000000, 0.6562500000000000000, 0.6875000000000000000, 0.7187500000000000000, 0.7500000000000000000, 0.7812500000000000000, 0.8125000000000000000, 0.8437500000000000000, 0.8750000000000000000, 0.9062500000000000000, 0.9375000000000000000, 0.9687500000000000000, 1.000000000000000000 ),
 .UNSPECIFIED. ) 
 GEOMETRIC_REPRESENTATION_ITEM ( )  RATIONAL_B_SPLINE_SURFACE ( (
 ( 1.000000000000000000, 0.9238795325112867385, 1.000000000000000000, 0.9238795325112867385, 1.000000000000000000, 0.9238795325112867385, 1.000000000000000000, 0.9238795325112867385, 1.000000000000000000, 0.9238795325112867385, 1.000000000000000000, 0.9238795325112867385, 1.000000000000000000, 0.9238795325112867385, 1.000000000000000000, 0.9238795325112867385, 1.000000000000000000, 0.9238795325112867385, 1.000000000000000000, 0.9238795325112867385, 1.000000000000000000, 0.9238795325112867385, 1.000000000000000000, 0.9238795325112867385, 1.000000000000000000, 0.9238795325112867385, 1.000000000000000000, 0.9238795325112867385, 1.000000000000000000, 0.9238795325112867385, 1.000000000000000000, 0.9238795325112867385, 1.000000000000000000, 0.9238795325112867385, 1.000000000000000000, 0.9238795325112867385, 1.000000000000000000, 0.9238795325112867385, 1.000000000000000000, 0.9238795325112867385, 1.000000000000000000, 0.9238795325112867385, 1.000000000000000000, 0.9238795325112867385, 1.000000000000000000, 0.9238795325112867385, 1.000000000000000000, 0.9238795325112867385, 1.000000000000000000, 0.9238795325112867385, 1.000000000000000000, 0.9238795325112867385, 1.000000000000000000, 0.9238795325112867385, 1.000000000000000000, 0.9238795325112867385, 1.000000000000000000, 0.9238795325112867385, 1.000000000000000000, 0.9238795325112867385, 1.000000000000000000, 0.9238795325112867385, 1.000000000000000000, 0.9238795325112867385, 1.000000000000000000),
 ( 1.000000000000000000, 0.9238795325112867385, 1.000000000000000000, 0.9238795325112867385, 1.000000000000000000, 0.9238795325112867385, 1.000000000000000000, 0.9238795325112867385, 1.000000000000000000, 0.9238795325112867385, 1.000000000000000000, 0.9238795325112867385, 1.000000000000000000, 0.9238795325112867385, 1.000000000000000000, 0.9238795325112867385, 1.000000000000000000, 0.9238795325112867385, 1.000000000000000000, 0.9238795325112867385, 1.000000000000000000, 0.9238795325112867385, 1.000000000000000000, 0.9238795325112867385, 1.000000000000000000, 0.9238795325112867385, 1.000000000000000000, 0.9238795325112867385, 1.000000000000000000, 0.9238795325112867385, 1.000000000000000000, 0.9238795325112867385, 1.000000000000000000, 0.9238795325112867385, 1.000000000000000000, 0.9238795325112867385, 1.000000000000000000, 0.9238795325112867385, 1.000000000000000000, 0.9238795325112867385, 1.000000000000000000, 0.9238795325112867385, 1.000000000000000000, 0.9238795325112867385, 1.000000000000000000, 0.9238795325112867385, 1.000000000000000000, 0.9238795325112867385, 1.000000000000000000, 0.9238795325112867385, 1.000000000000000000, 0.9238795325112867385, 1.000000000000000000, 0.9238795325112867385, 1.000000000000000000, 0.9238795325112867385, 1.000000000000000000, 0.9238795325112867385, 1.000000000000000000, 0.9238795325112867385, 1.000000000000000000, 0.9238795325112867385, 1.000000000000000000, 0.9238795325112867385, 1.000000000000000000) ) ) 
 REPRESENTATION_ITEM ( '' )  SURFACE ( )  );
#5075 = CYLINDRICAL_SURFACE ( 'NONE', #5461, 2.500000000000000444 ) ;
#5076 = CARTESIAN_POINT ( 'NONE',  ( 75.70742691175847483, 44.06379843619267689, -22.92955197636053555 ) ) ;
#5077 = CARTESIAN_POINT ( 'NONE',  ( -34.77260134704101802, 76.42358343581042845, 8.327459779344241753 ) ) ;
#5078 = ORIENTED_EDGE ( 'NONE', *, *, #9268, .T. ) ;
#5079 = CYLINDRICAL_SURFACE ( 'NONE', #11757, 30.00000000000000000 ) ;
#5080 = CARTESIAN_POINT ( 'NONE',  ( 71.95699135611712904, 10.32756980217126674, 21.14906888506658333 ) ) ;
#5081 = VECTOR ( 'NONE', #6929, 1000.000000000000000 ) ;
#5082 = EDGE_LOOP ( 'NONE', ( #5148, #6446, #9398, #10539 ) ) ;
#5083 = DIRECTION ( 'NONE',  ( 0.000000000000000000, 0.000000000000000000, -1.000000000000000000 ) ) ;
#5084 = EDGE_LOOP ( 'NONE', ( #10237, #9646, #8203, #4106 ) ) ;
#5085 = DIRECTION ( 'NONE',  ( 0.000000000000000000, 0.8660254037844405950, -0.4999999999999965028 ) ) ;
#5086 = CARTESIAN_POINT ( 'NONE',  ( 7.002289440008276244, 42.59914708353472435, 74.67617861058462836 ) ) ;
#5087 = VERTEX_POINT ( 'NONE', #9976 ) ;
#5088 = CARTESIAN_POINT ( 'NONE',  ( 0.000000000000000000, 285.0000000000000568, 0.000000000000000000 ) ) ;
#5089 = DIRECTION ( 'NONE',  ( 0.000000000000000000, 1.000000000000000000, 0.000000000000000000 ) ) ;
#5090 = DIRECTION ( 'NONE',  ( 0.000000000000000000, 0.000000000000000000, 1.000000000000000000 ) ) ;
#5091 = CARTESIAN_POINT ( 'NONE',  ( 3.061616997868383043E-15, 345.0000000000000568, -84.99999999999998579 ) ) ;
#5092 = AXIS2_PLACEMENT_3D ( 'NONE', #864, #929, #9383 ) ;
#5093 = TOROIDAL_SURFACE ( 'NONE', #9846, 12.99999999999999822, 2.000000000000000000 ) ;
#5094 = ORIENTED_EDGE ( 'NONE', *, *, #1377, .F. ) ;
#5095 = ORIENTED_EDGE ( 'NONE', *, *, #7266, .T. ) ;
#5096 = EDGE_CURVE ( 'NONE', #5565, #12345, #2293, .T. ) ;
#5097 = AXIS2_PLACEMENT_3D ( 'NONE', #3785, #5846, #11524 ) ;
#5098 = LINE ( 'NONE', #7884, #6894 ) ;
#5099 = DIRECTION ( 'NONE',  ( -0.000000000000000000, -1.000000000000000000, -0.000000000000000000 ) ) ;
#5100 = LINE ( 'NONE', #8882, #7798 ) ;
#5101 = AXIS2_PLACEMENT_3D ( 'NONE', #2829, #8430, #10366 ) ;
#5102 = AXIS2_PLACEMENT_3D ( 'NONE', #866, #6536, #8452 ) ;
#5103 = SURFACE_STYLE_FILL_AREA ( #7945 ) ;
#5104 = DIRECTION ( 'NONE',  ( -0.000000000000000000, 0.8660254037844402619, 0.4999999999999975575 ) ) ;
#5105 = FACE_OUTER_BOUND ( 'NONE', #7530, .T. ) ;
#5106 = CARTESIAN_POINT ( 'NONE',  ( -2.708734125000000770, 111.8749999986343937, -1.121994411437818639 ) ) ;
#5107 = CIRCLE ( 'NONE', #3299, 5.000000000000004441 ) ;
#5108 = ORIENTED_EDGE ( 'NONE', *, *, #1673, .T. ) ;
#5109 = DIRECTION ( 'NONE',  ( 0.000000000000000000, 1.000000000000000000, 0.000000000000000000 ) ) ;
#5110 = ADVANCED_FACE ( 'NONE', ( #11042 ), #9850, .F. ) ;
#5111 = EDGE_CURVE ( 'NONE', #10790, #9228, #2505, .T. ) ;
#5112 = AXIS2_PLACEMENT_3D ( 'NONE', #12142, #7460, #8259 ) ;
#5113 = VERTEX_POINT ( 'NONE', #3248 ) ;
#5114 = CARTESIAN_POINT ( 'NONE',  ( 0.000000000000000000, 153.0000000000000000, 2.099999999999998312 ) ) ;
#5115 = ORIENTED_EDGE ( 'NONE', *, *, #8199, .T. ) ;
#5116 = DIRECTION ( 'NONE',  ( 0.000000000000000000, 0.000000000000000000, -1.000000000000000000 ) ) ;
#5117 = LINE ( 'NONE', #361, #514 ) ;
#5118 = ORIENTED_EDGE ( 'NONE', *, *, #6953, .T. ) ;
#5119 = CARTESIAN_POINT ( 'NONE',  ( 0.000000000000000000, 170.0000000000000000, -15.00000000000000000 ) ) ;
#5120 = AXIS2_PLACEMENT_3D ( 'NONE', #10299, #8425, #1712 ) ;
#5121 = ADVANCED_FACE ( 'NONE', ( #5134 ), #11862, .F. ) ;
#5122 = DIRECTION ( 'NONE',  ( -0.000000000000000000, 1.000000000000000000, -0.000000000000000000 ) ) ;
#5123 = VERTEX_POINT ( 'NONE', #11989 ) ;
#5124 = CARTESIAN_POINT ( 'NONE',  ( -1.346194077712581150, 113.3125000000000000, 3.249999999999978240 ) ) ;
#5125 = EDGE_CURVE ( 'NONE', #8789, #9381, #9819, .T. ) ;
#5126 = AXIS2_PLACEMENT_3D ( 'NONE', #6433, #9155, #2444 ) ;
#5127 = ORIENTED_EDGE ( 'NONE', *, *, #9197, .T. ) ;
#5128 = CARTESIAN_POINT ( 'NONE',  ( 135.0000000000011084, 67.07106781186550393, 25.00000000000000000 ) ) ;
#5129 = DIRECTION ( 'NONE',  ( 0.000000000000000000, 0.000000000000000000, 1.000000000000000000 ) ) ;
#5130 = ORIENTED_EDGE ( 'NONE', *, *, #8900, .T. ) ;
#5131 = DIRECTION ( 'NONE',  ( 0.000000000000000000, 0.000000000000000000, 1.000000000000000000 ) ) ;
#5132 = CARTESIAN_POINT ( 'NONE',  ( 70.71510656582536569, 12.51027914909978733, 24.99160257227417148 ) ) ;
#5133 = EDGE_LOOP ( 'NONE', ( #3885, #6085, #251, #8023 ) ) ;
#5134 = FACE_OUTER_BOUND ( 'NONE', #8048, .T. ) ;
#5135 = EDGE_CURVE ( 'NONE', #4819, #6039, #9248, .T. ) ;
#5136 = CARTESIAN_POINT ( 'NONE',  ( 41.03553390593253170, -41.03553390593296513, -20.00000000000000000 ) ) ;
#5137 = CARTESIAN_POINT ( 'NONE',  ( -13.00000000000000178, 216.0365690573663926, -7.483314773547880883 ) ) ;
#5138 = ADVANCED_FACE ( 'NONE', ( #6061 ), #1325, .F. ) ;
#5139 = ORIENTED_EDGE ( 'NONE', *, *, #9128, .T. ) ;
#5140 = CARTESIAN_POINT ( 'NONE',  ( 142.0710678118665555, 59.99999999999998579, -25.00000000000000000 ) ) ;
#5141 = CARTESIAN_POINT ( 'NONE',  ( 69.92278643102456215, 15.49627177145660362, 27.12617897809031930 ) ) ;
#5142 = ORIENTED_EDGE ( 'NONE', *, *, #3601, .F. ) ;
#5143 = CARTESIAN_POINT ( 'NONE',  ( 77.45966692414835109, 15.00000000000008882, 20.00000000000000000 ) ) ;
#5144 = CARTESIAN_POINT ( 'NONE',  ( 70.75630133281138967, 47.58060937264504986, -24.87185742758410001 ) ) ;
#5145 = ORIENTED_EDGE ( 'NONE', *, *, #9887, .T. ) ;
#5146 = CARTESIAN_POINT ( 'NONE',  ( 0.000000000000000000, 110.0000000000000000, 0.000000000000000000 ) ) ;
#5147 = CARTESIAN_POINT ( 'NONE',  ( 72.18749001407745425, 45.14382420902206405, 20.39424303846705655 ) ) ;
#5148 = ORIENTED_EDGE ( 'NONE', *, *, #11274, .F. ) ;
#5149 = DIRECTION ( 'NONE',  ( -0.000000000000000000, -0.000000000000000000, 1.000000000000000000 ) ) ;
#5150 = CARTESIAN_POINT ( 'NONE',  ( -1.346194077712568049, 112.1874999972688016, 3.249999999999991118 ) ) ;
#5151 = EDGE_CURVE ( 'NONE', #8585, #3728, #9339, .T. ) ;
#5152 = CARTESIAN_POINT ( 'NONE',  ( 0.000000000000000000, 122.0000000000000000, 0.000000000000000000 ) ) ;
#5153 = DIRECTION ( 'NONE',  ( -0.7071067811865486830, -0.7071067811865464625, 0.000000000000000000 ) ) ;
#5154 = VECTOR ( 'NONE', #1990, 1000.000000000000114 ) ;
#5155 = STYLED_ITEM ( 'NONE', ( #77 ), #6166 ) ;
#5156 = EDGE_LOOP ( 'NONE', ( #4631, #11808, #6537, #4512 ) ) ;
#5157 = EDGE_LOOP ( 'NONE', ( #10734, #4850, #2696, #362 ) ) ;
#5158 = VERTEX_POINT ( 'NONE', #7488 ) ;
#5159 = DIRECTION ( 'NONE',  ( 0.000000000000000000, 0.000000000000000000, 1.000000000000000000 ) ) ;
#5160 = CARTESIAN_POINT ( 'NONE',  ( 0.000000000000000000, 115.0000000000000000, 0.000000000000000000 ) ) ;
#5161 = FACE_OUTER_BOUND ( 'NONE', #2804, .T. ) ;
#5162 = CARTESIAN_POINT ( 'NONE',  ( -1.041723228171368199, 45.00818216738166910, 74.99454991703274231 ) ) ;
#5163 = CARTESIAN_POINT ( 'NONE',  ( 2.500000000000000000, -2.357898499370432166, 3.035766082959412415E-15 ) ) ;
#5164 = CARTESIAN_POINT ( 'NONE',  ( -1.915364268218909150, 112.6874999986344079, 1.915364268218909594 ) ) ;
#5165 = ADVANCED_FACE ( 'NONE', ( #9216 ), #696, .F. ) ;
#5166 = ORIENTED_EDGE ( 'NONE', *, *, #3603, .F. ) ;
#5167 = FACE_BOUND ( 'NONE', #9826, .T. ) ;
#5168 = EDGE_CURVE ( 'NONE', #3622, #1438, #3259, .T. ) ;
#5169 = ORIENTED_EDGE ( 'NONE', *, *, #6540, .F. ) ;
#5170 = CARTESIAN_POINT ( 'NONE',  ( 27.02024436599224444, 275.0000000000000000, -111.3324139431193203 ) ) ;
#5171 = EDGE_LOOP ( 'NONE', ( #402, #6295, #6300, #2979 ) ) ;
#5172 = DIRECTION ( 'NONE',  ( -1.000000000000000000, 0.000000000000000000, -0.000000000000000000 ) ) ;
#5173 = CARTESIAN_POINT ( 'NONE',  ( 5.525725221640672480, 41.13333024919784719, 80.00000000000000000 ) ) ;
#5174 = EDGE_LOOP ( 'NONE', ( #2666, #6583, #7377, #9828 ) ) ;
#5175 = CIRCLE ( 'NONE', #12148, 98.00000000000001421 ) ;
#5176 = PLANE ( 'NONE',  #8433 ) ;
#5177 = CYLINDRICAL_SURFACE ( 'NONE', #10573, 5.000000000000000888 ) ;
#5178 = ADVANCED_FACE ( 'NONE', ( #4497 ), #11357, .T. ) ;
#5179 = ORIENTED_EDGE ( 'NONE', *, *, #4561, .F. ) ;
#5180 = CARTESIAN_POINT ( 'NONE',  ( -1.346194077712535409, 113.6875000000000000, -3.250000000000024869 ) ) ;
#5181 = EDGE_CURVE ( 'NONE', #9447, #11680, #5490, .T. ) ;
#5182 = VECTOR ( 'NONE', #5441, 1000.000000000000000 ) ;
#5183 = VERTEX_POINT ( 'NONE', #9400 ) ;
#5184 = CARTESIAN_POINT ( 'NONE',  ( 30.34950626935405182, 87.16600977219414403, 8.947791397837656646 ) ) ;
#5185 = FACE_OUTER_BOUND ( 'NONE', #9933, .T. ) ;
#5186 = ORIENTED_EDGE ( 'NONE', *, *, #10991, .F. ) ;
#5187 = CARTESIAN_POINT ( 'NONE',  ( 145.0000000000011369, 0.000000000000000000, -20.00000000000000000 ) ) ;
#5188 = DIRECTION ( 'NONE',  ( 0.000000000000000000, 0.000000000000000000, 1.000000000000000000 ) ) ;
#5189 = ORIENTED_EDGE ( 'NONE', *, *, #11515, .F. ) ;
#5190 = EDGE_CURVE ( 'NONE', #8715, #3552, #823, .T. ) ;
#5191 = DIRECTION ( 'NONE',  ( 0.000000000000000000, 1.000000000000000000, 0.000000000000000000 ) ) ;
#5192 = CARTESIAN_POINT ( 'NONE',  ( 74.16198487095665826, 40.36277934585979210, -25.00000000000000355 ) ) ;
#5193 = CARTESIAN_POINT ( 'NONE',  ( 3.592712519748626931, 21.21474596215575659, 79.50000000000000000 ) ) ;
#5194 = VECTOR ( 'NONE', #12088, 1000.000000000000000 ) ;
#5195 = ORIENTED_EDGE ( 'NONE', *, *, #1396, .T. ) ;
#5196 = CARTESIAN_POINT ( 'NONE',  ( 69.85388127645428824, 75.26794919243114634, -7.660254037844465458 ) ) ;
#5197 = AXIS2_PLACEMENT_3D ( 'NONE', #3147, #6951, #6019 ) ;
#5198 = CARTESIAN_POINT ( 'NONE',  ( 75.47338808840345337, 16.20969531357235027, 23.26499062814251317 ) ) ;
#5199 = VECTOR ( 'NONE', #4823, 1000.000000000000000 ) ;
#5200 = ORIENTED_EDGE ( 'NONE', *, *, #2952, .T. ) ;
#5201 = PRODUCT_DEFINITION ( 'UNKNOWN', '', #7344, #1275 ) ;
#5202 = CARTESIAN_POINT ( 'NONE',  ( 25.00000000000000000, 570.2996408614167194, -88.00000000000000000 ) ) ;
#5203 = DIRECTION ( 'NONE',  ( 0.000000000000000000, 0.000000000000000000, -1.000000000000000000 ) ) ;
#5204 = EDGE_LOOP ( 'NONE', ( #1908, #6125, #4930, #10213 ) ) ;
#5205 = FACE_OUTER_BOUND ( 'NONE', #9502, .T. ) ;
#5206 = CARTESIAN_POINT ( 'NONE',  ( 75.38891993288051196, 43.68400779952311552, 23.38442328187086616 ) ) ;
#5207 = EDGE_LOOP ( 'NONE', ( #6372, #558 ) ) ;
#5208 = DIRECTION ( 'NONE',  ( 0.000000000000000000, 0.4999999999999966138, 0.8660254037844407060 ) ) ;
#5209 = DIRECTION ( 'NONE',  ( 0.000000000000000000, 1.000000000000000000, 0.000000000000000000 ) ) ;
#5210 = SURFACE_STYLE_USAGE ( .BOTH. , #10809 ) ;
#5211 = CARTESIAN_POINT ( 'NONE',  ( -1.915364268218909816, 113.9374999986344079, -1.915364268218909150 ) ) ;
#5212 = AXIS2_PLACEMENT_3D ( 'NONE', #5187, #8967, #4362 ) ;
#5213 = AXIS2_PLACEMENT_3D ( 'NONE', #10780, #6167, #1492 ) ;
#5214 = EDGE_LOOP ( 'NONE', ( #8417, #4437, #1462, #9926 ) ) ;
#5215 = ORIENTED_EDGE ( 'NONE', *, *, #638, .T. ) ;
#5216 = EDGE_CURVE ( 'NONE', #10965, #4428, #1753, .T. ) ;
#5217 = CIRCLE ( 'NONE', #3614, 0.2000000000000000944 ) ;
#5218 = VECTOR ( 'NONE', #7523, 1000.000000000000000 ) ;
#5219 = CARTESIAN_POINT ( 'NONE',  ( 0.000000000000000000, 65.00000000000000000, -57.08203932499371547 ) ) ;
#5221 = EDGE_CURVE ( 'NONE', #3368, #8670, #5683, .T. ) ;
#5220 = LINE ( 'NONE', #7206, #4443 ) ;
#5222 = FACE_OUTER_BOUND ( 'NONE', #578, .T. ) ;
#5223 = CARTESIAN_POINT ( 'NONE',  ( 75.98513253586142469, 285.0000000000000568, 72.46557550663338532 ) ) ;
#5224 = DIRECTION ( 'NONE',  ( 0.000000000000000000, 0.000000000000000000, 1.000000000000000000 ) ) ;
#5225 = DIRECTION ( 'NONE',  ( 0.000000000000000000, 0.000000000000000000, 1.000000000000000000 ) ) ;
#5226 = DIRECTION ( 'NONE',  ( 1.000000000000000000, 0.000000000000000000, -0.000000000000000000 ) ) ;
#5227 = CARTESIAN_POINT ( 'NONE',  ( -1.915364268218909816, 113.9374999986344079, -1.915364268218909150 ) ) ;
#5228 = ORIENTED_EDGE ( 'NONE', *, *, #3630, .F. ) ;
#5229 = LINE ( 'NONE', #11903, #10954 ) ;
#5230 = ORIENTED_EDGE ( 'NONE', *, *, #7266, .F. ) ;
#5231 = DIRECTION ( 'NONE',  ( 0.000000000000000000, 0.5150380749100523792, 0.8571673007021134438 ) ) ;
#5232 = ORIENTED_EDGE ( 'NONE', *, *, #1021, .F. ) ;
#5233 = DIRECTION ( 'NONE',  ( 0.000000000000000000, 0.000000000000000000, 1.000000000000000000 ) ) ;
#5234 = CARTESIAN_POINT ( 'NONE',  ( 77.12313347048124967, 15.03062108036313482, -20.63522338802521006 ) ) ;
#5235 = EDGE_LOOP ( 'NONE', ( #5921, #7175, #12008, #11404 ) ) ;
#5236 = VECTOR ( 'NONE', #3264, 1000.000000000000000 ) ;
#5237 = LINE ( 'NONE', #6977, #10037 ) ;
#5238 = CARTESIAN_POINT ( 'NONE',  ( 117.9289321881355193, 45.00000000000008527, 20.00000000000000000 ) ) ;
#5239 = CONTEXT_DEPENDENT_SHAPE_REPRESENTATION ( #808, #415 ) ;
#5240 = EDGE_LOOP ( 'NONE', ( #4904, #2463, #2750, #563, #369 ) ) ;
#5241 = CARTESIAN_POINT ( 'NONE',  ( 70.88282142915603856, 47.91395231425131129, -24.51348554696366122 ) ) ;
#5242 = VECTOR ( 'NONE', #9071, 1000.000000000000000 ) ;
#5243 = ORIENTED_EDGE ( 'NONE', *, *, #10455, .T. ) ;
#5244 = ADVANCED_FACE ( 'NONE', ( #11300 ), #10406, .T. ) ;
#5245 = CYLINDRICAL_SURFACE ( 'NONE', #6533, 70.00000000000001421 ) ;
#5246 = DIRECTION ( 'NONE',  ( 0.000000000000000000, 0.000000000000000000, 1.000000000000000000 ) ) ;
#5247 = ORIENTED_EDGE ( 'NONE', *, *, #5007, .F. ) ;
#5248 = DIRECTION ( 'NONE',  ( -1.000000000000000000, 0.000000000000000000, 0.000000000000000000 ) ) ;
#5249 = CARTESIAN_POINT ( 'NONE',  ( 5.091510485526559826, 18.61875173514745185, 80.00000000000000000 ) ) ;
#5250 = VERTEX_POINT ( 'NONE', #12047 ) ;
#5251 = DIRECTION ( 'NONE',  ( 1.000000000000000000, 0.000000000000000000, 0.000000000000000000 ) ) ;
#5252 = CARTESIAN_POINT ( 'NONE',  ( 77.45966692414835109, 45.00000000000008527, -20.00000000000000000 ) ) ;
#5253 = LINE ( 'NONE', #507, #6800 ) ;
#5254 = VECTOR ( 'NONE', #10388, 1000.000000000000000 ) ;
#5255 = ORIENTED_EDGE ( 'NONE', *, *, #11486, .F. ) ;
#5256 = DIRECTION ( 'NONE',  ( 0.000000000000000000, 0.000000000000000000, -1.000000000000000000 ) ) ;
#5257 = CARTESIAN_POINT ( 'NONE',  ( 71.02603146012793900, 17.37440083699122795, 24.29862599233017662 ) ) ;
#5258 = EDGE_CURVE ( 'NONE', #5677, #4861, #5501, .T. ) ;
#5259 = EDGE_CURVE ( 'NONE', #4135, #1112, #7077, .T. ) ;
#5260 = ORIENTED_EDGE ( 'NONE', *, *, #3269, .T. ) ;
#5261 = FACE_OUTER_BOUND ( 'NONE', #5207, .T. ) ;
#5262 = DIRECTION ( 'NONE',  ( 0.000000000000000000, 0.000000000000000000, 1.000000000000000000 ) ) ;
#5263 = AXIS2_PLACEMENT_3D ( 'NONE', #11567, #1338, #10803 ) ;
#5264 = AXIS2_PLACEMENT_3D ( 'NONE', #2301, #8148, #4112 ) ;
#5265 = ORIENTED_EDGE ( 'NONE', *, *, #4213, .T. ) ;
#5266 = DIRECTION ( 'NONE',  ( -0.000000000000000000, -1.000000000000000000, -0.000000000000000000 ) ) ;
#5267 = CARTESIAN_POINT ( 'NONE',  ( 74.98782882127352423, 43.08750719129150752, 23.93624459205355137 ) ) ;
#5268 = ORIENTED_EDGE ( 'NONE', *, *, #8771, .T. ) ;
#5269 = FACE_OUTER_BOUND ( 'NONE', #9684, .T. ) ;
#5270 = CARTESIAN_POINT ( 'NONE',  ( 0.000000000000000000, 290.0000000000000568, 0.000000000000000000 ) ) ;
#5271 =( NAMED_UNIT ( * ) SI_UNIT ( $, .STERADIAN. ) SOLID_ANGLE_UNIT ( ) );
#5272 = CARTESIAN_POINT ( 'NONE',  ( 1.121994411437819084, 113.4999999986344079, 2.708734125000000326 ) ) ;
#5273 = EDGE_CURVE ( 'NONE', #2113, #1374, #4554, .T. ) ;
#5274 = EDGE_LOOP ( 'NONE', ( #6173, #9693, #8406, #7181 ) ) ;
#5275 = ORIENTED_EDGE ( 'NONE', *, *, #8275, .T. ) ;
#5276 = UNCERTAINTY_MEASURE_WITH_UNIT (LENGTH_MEASURE( 1.000000000000000082E-05 ), #5723, 'distance_accuracy_value', 'NONE');
#5277 = DIRECTION ( 'NONE',  ( -0.000000000000000000, 1.000000000000000000, 1.224646799147353207E-16 ) ) ;
#5278 = DIRECTION ( 'NONE',  ( 0.000000000000000000, 0.000000000000000000, -1.000000000000000000 ) ) ;
#5279 = CARTESIAN_POINT ( 'NONE',  ( 72.61843774138908714, 10.00000000000017586, -18.75000000000000000 ) ) ;
#5280 = CIRCLE ( 'NONE', #2681, 5.000000000000004441 ) ;
#5281 = CARTESIAN_POINT ( 'NONE',  ( 0.000000000000000000, 67.00000000000000000, 0.000000000000000000 ) ) ;
#5282 = AXIS2_PLACEMENT_3D ( 'NONE', #516, #10862, #9921 ) ;
#5283 = FACE_OUTER_BOUND ( 'NONE', #4299, .T. ) ;
#5284 = CARTESIAN_POINT ( 'NONE',  ( -75.98513253586240523, 275.0000000000000000, 72.46557550663233371 ) ) ;
#5285 = CARTESIAN_POINT ( 'NONE',  ( -14.19078112930533209, 29.75000000000008882, 80.00000000000000000 ) ) ;
#5286 = CARTESIAN_POINT ( 'NONE',  ( -1.190781129305471087, 30.00000000000008882, 65.00000000000000000 ) ) ;
#5287 = ADVANCED_FACE ( 'NONE', ( #8347 ), #12172, .T. ) ;
#5288 = ADVANCED_FACE ( 'NONE', ( #11233 ), #2562, .F. ) ;
#5289 = CARTESIAN_POINT ( 'NONE',  ( -1.121994411437820416, 112.9999999986343937, -2.708734124999999882 ) ) ;
#5290 = CARTESIAN_POINT ( 'NONE',  ( 1.915364268218909150, 110.6874999986344079, 1.915364268218909150 ) ) ;
#5291 = DIRECTION ( 'NONE',  ( 0.000000000000000000, 1.000000000000000000, 0.000000000000000000 ) ) ;
#5292 = AXIS2_PLACEMENT_3D ( 'NONE', #346, #11831, #4153 ) ;
#5293 = ORIENTED_EDGE ( 'NONE', *, *, #6485, .F. ) ;
#5294 = DIRECTION ( 'NONE',  ( 0.000000000000000000, 1.000000000000000000, 0.000000000000000000 ) ) ;
#5295 = ORIENTED_EDGE ( 'NONE', *, *, #4046, .T. ) ;
#5296 = CARTESIAN_POINT ( 'NONE',  ( 0.000000000000000000, 165.5000000000000000, 0.000000000000000000 ) ) ;
#5297 = CARTESIAN_POINT ( 'NONE',  ( 5.309218870694559556, 41.25833024919784719, 80.00000000000000000 ) ) ;
#5298 = VERTEX_POINT ( 'NONE', #6552 ) ;
#5299 = DIRECTION ( 'NONE',  ( 0.000000000000000000, 0.8660254037844405950, 0.4999999999999965028 ) ) ;
#5300 = LINE ( 'NONE', #2489, #12182 ) ;
#5301 = ITEM_DEFINED_TRANSFORMATION ( 'NONE', 'NONE', #1570,  #1612 ) ;
#5302 = ORIENTED_EDGE ( 'NONE', *, *, #348, .F. ) ;
#5303 = DIRECTION ( 'NONE',  ( 0.000000000000000000, 0.000000000000000000, 1.000000000000000000 ) ) ;
#5304 = ORIENTED_EDGE ( 'NONE', *, *, #8242, .T. ) ;
#5305 = DIRECTION ( 'NONE',  ( 0.000000000000000000, 0.000000000000000000, 1.000000000000000000 ) ) ;
#5306 = DIRECTION ( 'NONE',  ( 0.000000000000000000, 0.000000000000000000, 1.000000000000000000 ) ) ;
#5307 = VERTEX_POINT ( 'NONE', #6496 ) ;
#5308 = ORIENTED_EDGE ( 'NONE', *, *, #2430, .T. ) ;
#5309 = AXIS2_PLACEMENT_3D ( 'NONE', #212, #6644, #1905 ) ;
#5310 = FACE_OUTER_BOUND ( 'NONE', #3894, .T. ) ;
#5311 = DIRECTION ( 'NONE',  ( 1.049727191138621654E-16, 0.5150380749100502698, -0.8571673007021147761 ) ) ;
#5312 = ORIENTED_EDGE ( 'NONE', *, *, #2658, .T. ) ;
#5313 = DIRECTION ( 'NONE',  ( 1.000000000000000000, 0.000000000000000000, 0.000000000000000000 ) ) ;
#5314 = CARTESIAN_POINT ( 'NONE',  ( -0.9407811293052825707, 17.00000000000008882, 80.00000000000000000 ) ) ;
#5315 = CARTESIAN_POINT ( 'NONE',  ( 0.000000000000000000, 340.0000000000000000, 0.000000000000000000 ) ) ;
#5316 = ORIENTED_EDGE ( 'NONE', *, *, #2721, .T. ) ;
#5317 = CARTESIAN_POINT ( 'NONE',  ( 1.346194077712544956, 112.1875000000000142, 3.250000000000015543 ) ) ;
#5318 = EDGE_CURVE ( 'NONE', #5385, #938, #882, .T. ) ;
#5319 = CARTESIAN_POINT ( 'NONE',  ( 70.87894850892850229, 18.31681633891911787, 24.74065748999029779 ) ) ;
#5320 = CIRCLE ( 'NONE', #1932, 22.00000000000000355 ) ;
#5321 = EDGE_CURVE ( 'NONE', #3517, #3448, #6612, .T. ) ;
#5322 = VERTEX_POINT ( 'NONE', #6860 ) ;
#5323 = DIRECTION ( 'NONE',  ( -1.000000000000000000, 0.000000000000000000, -0.000000000000000000 ) ) ;
#5324 = DIRECTION ( 'NONE',  ( -0.000000000000000000, -1.000000000000000000, -0.000000000000000000 ) ) ;
#5325 = ORIENTED_EDGE ( 'NONE', *, *, #6897, .F. ) ;
#5326 = CARTESIAN_POINT ( 'NONE',  ( 63.96446609406733330, -63.96446609406769568, 20.00000000000000000 ) ) ;
#5327 = FACE_OUTER_BOUND ( 'NONE', #7005, .T. ) ;
#5328 = EDGE_LOOP ( 'NONE', ( #6807, #5450, #9890, #5831 ) ) ;
#5329 = CARTESIAN_POINT ( 'NONE',  ( 0.000000000000000000, 87.00000000000000000, 0.000000000000000000 ) ) ;
#5330 = CARTESIAN_POINT ( 'NONE',  ( -12.57411137850303540, 36.28349364905398033, 79.50000000000000000 ) ) ;
#5331 = CARTESIAN_POINT ( 'NONE',  ( -2.708734125000000326, 112.7499999986344079, 1.121994411437819084 ) ) ;
#5332 = EDGE_CURVE ( 'NONE', #4078, #6640, #4055, .T. ) ;
#5333 = ORIENTED_EDGE ( 'NONE', *, *, #582, .F. ) ;
#5334 =( NAMED_UNIT ( * ) PLANE_ANGLE_UNIT ( ) SI_UNIT ( $, .RADIAN. ) );
#5335 = EDGE_LOOP ( 'NONE', ( #772, #7737, #3714 ) ) ;
#5336 = FACE_OUTER_BOUND ( 'NONE', #8461, .T. ) ;
#5337 = DIRECTION ( 'NONE',  ( 0.000000000000000000, 0.000000000000000000, 1.000000000000000000 ) ) ;
#5338 = CARTESIAN_POINT ( 'NONE',  ( -34.73110591274434000, 77.00000000000000000, 8.660254037844445918 ) ) ;
#5339 = LINE ( 'NONE', #792, #6805 ) ;
#5340 = DIRECTION ( 'NONE',  ( -0.000000000000000000, -0.000000000000000000, 1.000000000000000000 ) ) ;
#5341 = CARTESIAN_POINT ( 'NONE',  ( 1.734723475976807094E-14, 63.00000000000000000, 57.08203932499370836 ) ) ;
#5342 = VECTOR ( 'NONE', #12346, 1000.000000000000114 ) ;
#5343 = CARTESIAN_POINT ( 'NONE',  ( 2.571758278209439492E-16, 153.0000000000000000, -2.099999999999998312 ) ) ;
#5344 = EDGE_CURVE ( 'NONE', #2311, #1312, #8656, .T. ) ;
#5345 = ADVANCED_FACE ( 'NONE', ( #6735 ), #12324, .T. ) ;
#5346 = CARTESIAN_POINT ( 'NONE',  ( 69.52686081652184669, 20.00000000000009237, -28.12499999999999645 ) ) ;
#5347 = CARTESIAN_POINT ( 'NONE',  ( -2.298097038856279362, 113.3750000000000000, 2.298097038856279806 ) ) ;
#5348 = VERTEX_POINT ( 'NONE', #7607 ) ;
#5349 = DIRECTION ( 'NONE',  ( -0.000000000000000000, 1.000000000000000000, -0.000000000000000000 ) ) ;
#5350 = VECTOR ( 'NONE', #8126, 1000.000000000000114 ) ;
#5351 = PRODUCT_DEFINITION_FORMATION_WITH_SPECIFIED_SOURCE ( 'ANY', '', #9761, .NOT_KNOWN. ) ;
#5352 = LINE ( 'NONE', #4533, #9775 ) ;
#5353 = ORIENTED_EDGE ( 'NONE', *, *, #2087, .F. ) ;
#5354 = DIRECTION ( 'NONE',  ( 0.8660254037844385966, -0.5000000000000000000, 0.000000000000000000 ) ) ;
#5355 = ORIENTED_EDGE ( 'NONE', *, *, #6897, .T. ) ;
#5356 = DIRECTION ( 'NONE',  ( -1.000000000000000000, 0.000000000000000000, -0.000000000000000000 ) ) ;
#5357 = DIRECTION ( 'NONE',  ( 0.000000000000000000, 0.000000000000000000, -1.000000000000000000 ) ) ;
#5358 = ORIENTED_EDGE ( 'NONE', *, *, #3103, .F. ) ;
#5359 = DIRECTION ( 'NONE',  ( -0.7071067811865454633, 0.7071067811865495711, 0.000000000000000000 ) ) ;
#5360 = LINE ( 'NONE', #10962, #6164 ) ;
#5361 = EDGE_LOOP ( 'NONE', ( #10017, #11912, #2484, #7441 ) ) ;
#5362 = CARTESIAN_POINT ( 'NONE',  ( 69.90350624952219505, 44.39669317652923297, -27.17578603812305360 ) ) ;
#5363 = VERTEX_POINT ( 'NONE', #11544 ) ;
#5364 = EDGE_CURVE ( 'NONE', #4409, #8712, #5684, .T. ) ;
#5365 = CARTESIAN_POINT ( 'NONE',  ( 29.94260118448502794, 78.56931597186009242, -5.428213010295147356 ) ) ;
#5366 = CIRCLE ( 'NONE', #9934, 4.250000000000000000 ) ;
#5367 = CARTESIAN_POINT ( 'NONE',  ( -1.346194077712535409, 114.5624999972688158, -3.250000000000024869 ) ) ;
#5368 = VERTEX_POINT ( 'NONE', #243 ) ;
#5369 = VECTOR ( 'NONE', #4878, 1000.000000000000000 ) ;
#5370 = CARTESIAN_POINT ( 'NONE',  ( 0.000000000000000000, 265.0000000000000000, 0.000000000000000000 ) ) ;
#5371 = CARTESIAN_POINT ( 'NONE',  ( 0.000000000000000000, 65.00000000000000000, 0.000000000000000000 ) ) ;
#5372 = VERTEX_POINT ( 'NONE', #1191 ) ;
#5373 = DIRECTION ( 'NONE',  ( 0.000000000000000000, 0.000000000000000000, 1.000000000000000000 ) ) ;
#5374 = CARTESIAN_POINT ( 'NONE',  ( -24.76446302067273209, 285.0000000000000568, -102.0378428393002679 ) ) ;
#5375 = CARTESIAN_POINT ( 'NONE',  ( 11.80921887069467324, 30.25000000000018474, 79.50000000000000000 ) ) ;
#5376 = VERTEX_POINT ( 'NONE', #3993 ) ;
#5377 = CARTESIAN_POINT ( 'NONE',  ( 3.250000000000000444, 112.0624999999999858, 1.346194077712559167 ) ) ;
#5378 = CARTESIAN_POINT ( 'NONE',  ( 0.000000000000000000, 110.0000000000000000, 0.000000000000000000 ) ) ;
#5379 = AXIS2_PLACEMENT_3D ( 'NONE', #1859, #12282, #5672 ) ;
#5380 = AXIS2_PLACEMENT_3D ( 'NONE', #4010, #2886, #6695 ) ;
#5381 = ORIENTED_EDGE ( 'NONE', *, *, #11242, .T. ) ;
#5382 = EDGE_CURVE ( 'NONE', #5829, #5123, #8846, .T. ) ;
#5383 = DIRECTION ( 'NONE',  ( 0.000000000000000000, -1.000000000000000000, -0.000000000000000000 ) ) ;
#5384 = DIRECTION ( 'NONE',  ( 0.000000000000000000, 1.000000000000000000, 0.000000000000000000 ) ) ;
#5385 = VERTEX_POINT ( 'NONE', #6921 ) ;
#5386 = CYLINDRICAL_SURFACE ( 'NONE', #6652, 4.999999999999997335 ) ;
#5387 = CARTESIAN_POINT ( 'NONE',  ( 70.67711243716091474, 47.36801559909221737, 25.09579365358156622 ) ) ;
#5388 = VERTEX_POINT ( 'NONE', #2936 ) ;
#5389 = CARTESIAN_POINT ( 'NONE',  ( -25.00000000000000000, 445.0000000000000568, -88.00000000000000000 ) ) ;
#5390 = EDGE_CURVE ( 'NONE', #8667, #4721, #7666, .T. ) ;
#5391 = DIRECTION ( 'NONE',  ( 0.000000000000000000, 1.000000000000000000, 0.000000000000000000 ) ) ;
#5392 = CARTESIAN_POINT ( 'NONE',  ( -2.708734125000000770, 113.8749999986344079, -1.121994411437818639 ) ) ;
#5393 = CARTESIAN_POINT ( 'NONE',  ( 1.121994411437819084, 112.3749999986344221, -2.708734124999999437 ) ) ;
#5394 = ORIENTED_EDGE ( 'NONE', *, *, #9547, .F. ) ;
#5395 =( BOUNDED_CURVE ( )  B_SPLINE_CURVE ( 2, ( #291, #3980, #1053, #995, #11595, #5045, #4044, #6847, #6784 ),
 .UNSPECIFIED., .F., .F. ) 
 B_SPLINE_CURVE_WITH_KNOTS ( ( 3, 2, 2, 2, 3 ),
 ( 0.5625000000000004441, 0.5937500000000004441, 0.6250000000000004441, 0.6562500000000005551, 0.6875000000000005551 ),
 .UNSPECIFIED. ) 
 CURVE ( )  GEOMETRIC_REPRESENTATION_ITEM ( )  RATIONAL_B_SPLINE_CURVE ( ( 0.9999999999999988898, 0.9238795325112878487, 1.000000000000000000, 0.9238795325112867385, 1.000000000000000000, 0.9238795325112867385, 1.000000000000000000, 0.9238795325112854062, 1.000000000000001332 ) ) 
 REPRESENTATION_ITEM ( '' )  );
#5396 = EDGE_LOOP ( 'NONE', ( #11610, #8502 ) ) ;
#5397 =( NAMED_UNIT ( * ) PLANE_ANGLE_UNIT ( ) SI_UNIT ( $, .RADIAN. ) );
#5398 = AXIS2_PLACEMENT_3D ( 'NONE', #12251, #8547, #784 ) ;
#5399 = STYLED_ITEM ( 'NONE', ( #11456 ), #10022 ) ;
#5400 = DIRECTION ( 'NONE',  ( 0.000000000000000000, -1.224646799147353454E-16, 1.000000000000000000 ) ) ;
#5401 = DIRECTION ( 'NONE',  ( -1.000000000000000000, -0.000000000000000000, -0.000000000000000000 ) ) ;
#5402 = EDGE_CURVE ( 'NONE', #4828, #11220, #3858, .T. ) ;
#5403 = EDGE_CURVE ( 'NONE', #6450, #9081, #8655, .T. ) ;
#5404 = LINE ( 'NONE', #9118, #1651 ) ;
#5405 = CARTESIAN_POINT ( 'NONE',  ( 0.000000000000000000, 275.0000000000000000, 0.000000000000000000 ) ) ;
#5406 = DIRECTION ( 'NONE',  ( -0.000000000000000000, -0.000000000000000000, 1.000000000000000000 ) ) ;
#5407 = AXIS2_PLACEMENT_3D ( 'NONE', #8349, #7609, #12175 ) ;
#5408 = DIRECTION ( 'NONE',  ( 0.000000000000000000, 0.000000000000000000, 1.000000000000000000 ) ) ;
#5409 = LINE ( 'NONE', #2594, #4404 ) ;
#5410 = CARTESIAN_POINT ( 'NONE',  ( 3.249999999999999556, 111.8124999972688016, -1.346194077712561166 ) ) ;
#5411 = VERTEX_POINT ( 'NONE', #11665 ) ;
#5412 = CARTESIAN_POINT ( 'NONE',  ( -3.250000000000000444, 112.4375000000000000, 1.346194077712559389 ) ) ;
#5413 = DIRECTION ( 'NONE',  ( -0.000000000000000000, -1.000000000000000000, -0.000000000000000000 ) ) ;
#5414 = AXIS2_PLACEMENT_3D ( 'NONE', #1443, #8034, #7050 ) ;
#5415 = EDGE_CURVE ( 'NONE', #5952, #12245, #3116, .T. ) ;
#5416 = ADVANCED_FACE ( 'NONE', ( #1006 ), #11483, .T. ) ;
#5417 = FACE_OUTER_BOUND ( 'NONE', #6046, .T. ) ;
#5418 = ORIENTED_EDGE ( 'NONE', *, *, #8645, .F. ) ;
#5419 = DIRECTION ( 'NONE',  ( 0.000000000000000000, 0.000000000000000000, 1.000000000000000000 ) ) ;
#5420 = DIRECTION ( 'NONE',  ( 0.000000000000000000, 0.000000000000000000, -1.000000000000000000 ) ) ;
#5421 = CARTESIAN_POINT ( 'NONE',  ( 117.9289321881355193, 50.00000000000008527, -19.99999999999999645 ) ) ;
#5422 = ORIENTED_EDGE ( 'NONE', *, *, #6955, .T. ) ;
#5423 = LINE ( 'NONE', #619, #11032 ) ;
#5424 = DIRECTION ( 'NONE',  ( 0.000000000000000000, 1.000000000000000000, 0.000000000000000000 ) ) ;
#5425 = EDGE_LOOP ( 'NONE', ( #7116, #7542, #10605, #802 ) ) ;
#5426 = CARTESIAN_POINT ( 'NONE',  ( -6.407287480251453893, 38.53525403784446723, 79.50000000000000000 ) ) ;
#5427 = VERTEX_POINT ( 'NONE', #2124 ) ;
#5428 = EDGE_LOOP ( 'NONE', ( #111, #10454, #2833, #647 ) ) ;
#5429 = AXIS2_PLACEMENT_3D ( 'NONE', #3587, #6396, #1596 ) ;
#5430 = CARTESIAN_POINT ( 'NONE',  ( 30.99900678938364251, 76.83479030960515388, -8.564870178622241426 ) ) ;
#5431 = CARTESIAN_POINT ( 'NONE',  ( 0.000000000000000000, 87.00000000000000000, 0.000000000000000000 ) ) ;
#5432 = ORIENTED_EDGE ( 'NONE', *, *, #3831, .F. ) ;
#5433 = CARTESIAN_POINT ( 'NONE',  ( 5.309218870694537351, 18.74166975080233044, 80.00000000000000000 ) ) ;
#5434 = DIRECTION ( 'NONE',  ( -1.000000000000000000, 0.000000000000000000, 3.469446951953613203E-16 ) ) ;
#5435 = ORIENTED_EDGE ( 'NONE', *, *, #9564, .F. ) ;
#5436 = DIRECTION ( 'NONE',  ( 1.000000000000000000, 0.000000000000000000, 0.000000000000000000 ) ) ;
#5437 = DIRECTION ( 'NONE',  ( 0.000000000000000000, 0.000000000000000000, 1.000000000000000000 ) ) ;
#5438 = CARTESIAN_POINT ( 'NONE',  ( 3.250000000000000444, 110.4374999986344079, 0.000000000000000000 ) ) ;
#5439 = DIRECTION ( 'NONE',  ( -0.000000000000000000, -1.000000000000000000, -0.000000000000000000 ) ) ;
#5440 = VERTEX_POINT ( 'NONE', #5987 ) ;
#5441 = DIRECTION ( 'NONE',  ( 0.000000000000000000, -0.8660254037844405950, 0.4999999999999965028 ) ) ;
#5442 = EDGE_CURVE ( 'NONE', #8327, #1960, #1300, .T. ) ;
#5443 = ADVANCED_FACE ( 'NONE', ( #8717 ), #8257, .T. ) ;
#5444 = CIRCLE ( 'NONE', #10011, 5.000000000000000000 ) ;
#5445 = LINE ( 'NONE', #9223, #4595 ) ;
#5446 = ADVANCED_FACE ( 'NONE', ( #2867 ), #6673, .T. ) ;
#5447 = ORIENTED_EDGE ( 'NONE', *, *, #11534, .F. ) ;
#5448 = LINE ( 'NONE', #11245, #6957 ) ;
#5449 = DIRECTION ( 'NONE',  ( -1.776356839400250465E-15, 0.000000000000000000, 1.000000000000000000 ) ) ;
#5450 = ORIENTED_EDGE ( 'NONE', *, *, #9367, .T. ) ;
#5451 = CARTESIAN_POINT ( 'NONE',  ( 0.000000000000000000, 265.0000000000000000, 0.000000000000000000 ) ) ;
#5452 = LINE ( 'NONE', #8482, #2300 ) ;
#5453 = AXIS2_PLACEMENT_3D ( 'NONE', #1350, #1474, #5159 ) ;
#5454 = ORIENTED_EDGE ( 'NONE', *, *, #6310, .F. ) ;
#5455 = CARTESIAN_POINT ( 'NONE',  ( 25.00000000000000000, 345.0000000000000568, -59.99999999999999289 ) ) ;
#5456 = DIRECTION ( 'NONE',  ( -0.000000000000000000, -1.000000000000000000, -0.000000000000000000 ) ) ;
#5457 = CARTESIAN_POINT ( 'NONE',  ( 2.143131898507868248E-15, 127.0000000000000000, 17.50000000000000000 ) ) ;
#5458 = CARTESIAN_POINT ( 'NONE',  ( 2.708734124999999882, 111.6249999986344079, 1.121994411437818862 ) ) ;
#5459 = EDGE_LOOP ( 'NONE', ( #847, #4501, #2660, #9047, #4797, #7533, #3721 ) ) ;
#5460 = VECTOR ( 'NONE', #1536, 1000.000000000000000 ) ;
#5461 = AXIS2_PLACEMENT_3D ( 'NONE', #4127, #10312, #5762 ) ;
#5462 = CARTESIAN_POINT ( 'NONE',  ( 10.19254911989230727, 36.28349364905406560, 80.00000000000000000 ) ) ;
#5463 = CARTESIAN_POINT ( 'NONE',  ( -24.99999999999999645, 450.0000000000000568, -105.0000000000000000 ) ) ;
#5464 = CARTESIAN_POINT ( 'NONE',  ( -34.17938886450476588, 77.00000000000000000, 8.633741422215349459 ) ) ;
#5465 = CARTESIAN_POINT ( 'NONE',  ( 3.061616997868383043E-15, 75.00000000000001421, -25.00000000000000000 ) ) ;
#5466 = CARTESIAN_POINT ( 'NONE',  ( -29.05832229253449128, 87.09380371750548022, -8.606096436291647223 ) ) ;
#5467 = DIRECTION ( 'NONE',  ( -1.000000000000000000, -0.000000000000000000, -0.000000000000000000 ) ) ;
#5468 = CARTESIAN_POINT ( 'NONE',  ( 12.60805306350328969, 24.10018532896172516, 73.93285131058543413 ) ) ;
#5469 = VECTOR ( 'NONE', #7442, 1000.000000000000227 ) ;
#5470 = VERTEX_POINT ( 'NONE', #9524 ) ;
#5471 = B_SPLINE_CURVE_WITH_KNOTS ( 'NONE', 3,
 ( #7409, #4592, #11086, #10317, #2722, #2542, #1608, #7468, #6531, #1787, #5600, #3472, #472, #4399, #4281, #10008, #736, #7338, #5468, #8194, #1602, #9252, #8073, #12084, #10066, #9123 ),
 .UNSPECIFIED., .F., .F.,
 ( 4, 2, 2, 2, 2, 2, 2, 2, 2, 2, 2, 2, 4 ),
 ( 1.022432916270031883E-18, 0.002788363146399075020, 0.004182544719598612314, 0.005576726292798150041, 0.008365089439197226362, 0.009759271012396762354, 0.01115345258559629835, 0.01394181573199535992, 0.01533599730519489591, 0.01673017887839442844, 0.01951854202479350042, 0.02091272359799303121, 0.02230690517119256200 ),
 .UNSPECIFIED. ) ;
#5472 = TOROIDAL_SURFACE ( 'NONE', #12246, 4.000000000000000000, 0.2500000000000000000 ) ;
#5473 = CARTESIAN_POINT ( 'NONE',  ( 1.346194077712559833, 113.8125000000000000, -3.250000000000000000 ) ) ;
#5474 = CARTESIAN_POINT ( 'NONE',  ( 2.081899558550500280E-15, 75.00000000000001421, 17.00000000000000000 ) ) ;
#5475 = ADVANCED_FACE ( 'NONE', ( #4802, #8592 ), #53, .T. ) ;
#5476 = AXIS2_PLACEMENT_3D ( 'NONE', #7712, #98, #10389 ) ;
#5477 = CARTESIAN_POINT ( 'NONE',  ( -0.9407811293054709756, 43.00000000000008527, 80.00000000000000000 ) ) ;
#5478 = CIRCLE ( 'NONE', #8047, 5.000000000000000888 ) ;
#5479 = ORIENTED_EDGE ( 'NONE', *, *, #10585, .T. ) ;
#5480 = DIRECTION ( 'NONE',  ( 0.000000000000000000, 1.000000000000000000, 0.000000000000000000 ) ) ;
#5481 = PLANE ( 'NONE',  #5102 ) ;
#5482 = EDGE_LOOP ( 'NONE', ( #9904, #10437, #11958, #5588, #21 ) ) ;
#5483 = CARTESIAN_POINT ( 'NONE',  ( 25.00000000000000355, 345.0000000000000568, -90.00000000000000000 ) ) ;
#5484 = DIRECTION ( 'NONE',  ( -0.000000000000000000, -1.000000000000000000, -0.000000000000000000 ) ) ;
#5485 = EDGE_CURVE ( 'NONE', #298, #5411, #6851, .T. ) ;
#5486 = AXIS2_PLACEMENT_3D ( 'NONE', #5885, #5820, #9605 ) ;
#5487 = VERTEX_POINT ( 'NONE', #1249 ) ;
#5488 = EDGE_CURVE ( 'NONE', #7769, #1834, #4231, .T. ) ;
#5489 = DIRECTION ( 'NONE',  ( -0.000000000000000000, -0.000000000000000000, 1.000000000000000000 ) ) ;
#5490 = CIRCLE ( 'NONE', #95, 95.00000000000002842 ) ;
#5491 = EDGE_LOOP ( 'NONE', ( #8910, #3263, #5940, #4286 ) ) ;
#5492 = CARTESIAN_POINT ( 'NONE',  ( 0.000000000000000000, 115.0000000000000000, -15.00000000000000000 ) ) ;
#5494 = VERTEX_POINT ( 'NONE', #11851 ) ;
#5493 = DIRECTION ( 'NONE',  ( 0.000000000000000000, 0.000000000000000000, -1.000000000000000000 ) ) ;
#5495 = EDGE_LOOP ( 'NONE', ( #961, #591, #8838, #5936 ) ) ;
#5496 = VECTOR ( 'NONE', #10358, 999.9999999999998863 ) ;
#5497 = DIRECTION ( 'NONE',  ( -0.000000000000000000, -1.000000000000000000, -0.000000000000000000 ) ) ;
#5498 = CARTESIAN_POINT ( 'NONE',  ( -30.99900678938364251, 76.83479030960515388, 8.564870178622241426 ) ) ;
#5499 = ORIENTED_EDGE ( 'NONE', *, *, #248, .T. ) ;
#5500 = DIRECTION ( 'NONE',  ( 0.000000000000000000, 0.000000000000000000, 1.000000000000000000 ) ) ;
#5501 = LINE ( 'NONE', #764, #4256 ) ;
#5502 = AXIS2_PLACEMENT_3D ( 'NONE', #11414, #6323, #12063 ) ;
#5503 = CARTESIAN_POINT ( 'NONE',  ( 17.30235457177317571, 275.0000000000000000, -113.6909342308024407 ) ) ;
#5504 = CARTESIAN_POINT ( 'NONE',  ( 2.298097038856279806, 110.9999999972688158, 2.298097038856279806 ) ) ;
#5505 = ADVANCED_FACE ( 'NONE', ( #3429 ), #9774, .F. ) ;
#5506 = ADVANCED_FACE ( 'NONE', ( #11790 ), #5176, .F. ) ;
#5507 = VERTEX_POINT ( 'NONE', #5119 ) ;
#5508 = CARTESIAN_POINT ( 'NONE',  ( -4.975863863883684959E-16, 111.3124999986344079, -2.708734124999999882 ) ) ;
#5509 = CARTESIAN_POINT ( 'NONE',  ( -6.407287480251391720, 21.46474596215567487, 79.50000000000000000 ) ) ;
#5510 = APPLICATION_CONTEXT ( 'automotive_design' ) ;
#5511 = AXIS2_PLACEMENT_3D ( 'NONE', #5371, #12290, #11104 ) ;
#5512 = VECTOR ( 'NONE', #149, 1000.000000000000000 ) ;
#5513 = EDGE_LOOP ( 'NONE', ( #8301, #4761, #1164, #279 ) ) ;
#5514 = CARTESIAN_POINT ( 'NONE',  ( -11.19078112930532853, 29.75000000000005684, 79.50000000000000000 ) ) ;
#5515 = CARTESIAN_POINT ( 'NONE',  ( 145.0000000000011369, 67.07106781186550393, -25.00000000000000000 ) ) ;
#5516 = ORIENTED_EDGE ( 'NONE', *, *, #10379, .F. ) ;
#5517 = CYLINDRICAL_SURFACE ( 'NONE', #3871, 3.250000000000000444 ) ;
#5518 = CARTESIAN_POINT ( 'NONE',  ( 72.45821416003295212, 45.13374170404204477, 19.37058730516574556 ) ) ;
#5519 = ORIENTED_EDGE ( 'NONE', *, *, #7271, .T. ) ;
#5520 = EDGE_CURVE ( 'NONE', #6241, #3797, #1169, .T. ) ;
#5521 = DIRECTION ( 'NONE',  ( 0.000000000000000000, 1.000000000000000000, -1.287488025362403787E-15 ) ) ;
#5522 = CARTESIAN_POINT ( 'NONE',  ( 34.84121487603211875, 75.26794919243111792, -7.660254037844449471 ) ) ;
#5523 = CARTESIAN_POINT ( 'NONE',  ( 2.708734124999999882, 110.6249999986343937, 1.121994411437818862 ) ) ;
#5524 = AXIS2_PLACEMENT_3D ( 'NONE', #8364, #9171, #2639 ) ;
#5525 = VERTEX_POINT ( 'NONE', #11970 ) ;
#5526 = ORIENTED_EDGE ( 'NONE', *, *, #2952, .F. ) ;
#5527 = CARTESIAN_POINT ( 'NONE',  ( 13.80921887069452758, 30.00000000000009237, 75.00000000000001421 ) ) ;
#5528 = EDGE_CURVE ( 'NONE', #6671, #3140, #9021, .T. ) ;
#5529 = DIRECTION ( 'NONE',  ( -0.000000000000000000, 1.000000000000000000, -0.000000000000000000 ) ) ;
#5530 = CARTESIAN_POINT ( 'NONE',  ( -30.43737458073258040, 77.00000000000001421, 5.702507482421638407 ) ) ;
#5531 = PLANE ( 'NONE',  #12162 ) ;
#5532 = CARTESIAN_POINT ( 'NONE',  ( -27.32044479829590244, 86.95653975047672191, -12.39329872843003066 ) ) ;
#5533 = CARTESIAN_POINT ( 'NONE',  ( -15.63374382699839948, 34.08284429348438493, 73.35265631139654374 ) ) ;
#5534 = PLANE ( 'NONE',  #5026 ) ;
#5535 = VERTEX_POINT ( 'NONE', #2488 ) ;
#5536 = CARTESIAN_POINT ( 'NONE',  ( -3.250000000000000444, 112.5000000000000000, 3.980102097228898231E-16 ) ) ;
#5537 = CARTESIAN_POINT ( 'NONE',  ( 1.163414459189985801E-14, 65.00000000000000000, -90.00000000000002842 ) ) ;
#5538 = CARTESIAN_POINT ( 'NONE',  ( 1.102182119232618227E-14, 75.00000000000001421, -90.00000000000002842 ) ) ;
#5539 = ORIENTED_EDGE ( 'NONE', *, *, #4910, .F. ) ;
#5540 = EDGE_CURVE ( 'NONE', #298, #5087, #10961, .T. ) ;
#5541 = AXIS2_PLACEMENT_3D ( 'NONE', #3676, #7482, #11294 ) ;
#5542 = CARTESIAN_POINT ( 'NONE',  ( -25.00000000000000000, 345.0000000000000568, -95.00000000000000000 ) ) ;
#5543 = DIRECTION ( 'NONE',  ( -1.000000000000000000, 0.000000000000000000, -0.000000000000000000 ) ) ;
#5544 = CARTESIAN_POINT ( 'NONE',  ( 69.52686081652184669, 20.00000000000008882, -28.12499999999999645 ) ) ;
#5545 = ORIENTED_EDGE ( 'NONE', *, *, #10347, .T. ) ;
#5546 = EDGE_CURVE ( 'NONE', #12245, #2361, #3665, .T. ) ;
#5547 = FACE_OUTER_BOUND ( 'NONE', #7793, .T. ) ;
#5548 = EDGE_CURVE ( 'NONE', #6039, #8739, #474, .T. ) ;
#5549 = DIRECTION ( 'NONE',  ( 0.000000000000000000, 0.000000000000000000, 1.000000000000000000 ) ) ;
#5550 = ORIENTED_EDGE ( 'NONE', *, *, #8649, .F. ) ;
#5551 = CYLINDRICAL_SURFACE ( 'NONE', #6375, 4.250000000000000000 ) ;
#5552 = AXIS2_PLACEMENT_3D ( 'NONE', #4456, #9936, #7205 ) ;
#5553 = PRESENTATION_LAYER_ASSIGNMENT (  '', '', ( #10913 ) ) ;
#5554 = ORIENTED_EDGE ( 'NONE', *, *, #6608, .F. ) ;
#5555 = DIRECTION ( 'NONE',  ( 0.000000000000000000, 0.000000000000000000, 1.000000000000000000 ) ) ;
#5556 = DIRECTION ( 'NONE',  ( 0.000000000000000000, 1.000000000000000000, 0.000000000000000000 ) ) ;
#5557 = EDGE_LOOP ( 'NONE', ( #1710, #11906, #8241, #11166 ) ) ;
#5558 = DIRECTION ( 'NONE',  ( 0.000000000000000000, 1.000000000000000000, 0.000000000000000000 ) ) ;
#5559 = ORIENTED_EDGE ( 'NONE', *, *, #10096, .T. ) ;
#5560 = EDGE_CURVE ( 'NONE', #4906, #9416, #7102, .T. ) ;
#5561 = EDGE_CURVE ( 'NONE', #7137, #1550, #9825, .T. ) ;
#5562 = DIRECTION ( 'NONE',  ( 0.000000000000000000, 1.000000000000000000, 0.000000000000000000 ) ) ;
#5563 = DIRECTION ( 'NONE',  ( 0.000000000000000000, 1.000000000000000000, 0.000000000000000000 ) ) ;
#5564 = CARTESIAN_POINT ( 'NONE',  ( -27.02024436599226576, 275.0000000000000000, -111.3324139431193345 ) ) ;
#5565 = VERTEX_POINT ( 'NONE', #4169 ) ;
#5566 = CARTESIAN_POINT ( 'NONE',  ( 1.121994411437819084, 113.3749999986344079, -2.708734124999999437 ) ) ;
#5567 = ADVANCED_FACE ( 'NONE', ( #8836 ), #9958, .T. ) ;
#5568 = CARTESIAN_POINT ( 'NONE',  ( 3.980102097228898231E-16, 110.0000000000000000, -3.250000000000000444 ) ) ;
#5569 = CIRCLE ( 'NONE', #1409, 24.99999999999999645 ) ;
#5570 = VERTEX_POINT ( 'NONE', #428 ) ;
#5571 = DIRECTION ( 'NONE',  ( -1.000000000000000000, 0.000000000000000000, -6.938893903907228378E-17 ) ) ;
#5572 = EDGE_CURVE ( 'NONE', #9412, #1574, #1432, .T. ) ;
#5573 = DIRECTION ( 'NONE',  ( 0.8660254037844434816, 0.4999999999999913958, 0.000000000000000000 ) ) ;
#5574 = EDGE_LOOP ( 'NONE', ( #331, #8186, #4655, #11529 ) ) ;
#5575 = CARTESIAN_POINT ( 'NONE',  ( 145.0000000000011369, 30.00000000000008882, 20.00000000000000000 ) ) ;
#5576 = DIRECTION ( 'NONE',  ( 0.000000000000000000, 0.000000000000000000, -1.000000000000000000 ) ) ;
#5577 = ORIENTED_EDGE ( 'NONE', *, *, #513, .T. ) ;
#5578 = DIRECTION ( 'NONE',  ( 0.5000000000000036637, 0.8660254037844365982, 0.000000000000000000 ) ) ;
#5579 = DIRECTION ( 'NONE',  ( -0.000000000000000000, -1.000000000000000000, -0.000000000000000000 ) ) ;
#5580 = VECTOR ( 'NONE', #2609, 1000.000000000000114 ) ;
#5581 = CARTESIAN_POINT ( 'NONE',  ( -2.708734124999999882, 112.9999999986343937, 1.121994411437818862 ) ) ;
#5582 = DIRECTION ( 'NONE',  ( 1.000000000000000000, -0.000000000000000000, 1.564230817409691233E-15 ) ) ;
#5583 = ORIENTED_EDGE ( 'NONE', *, *, #973, .F. ) ;
#5584 = SHAPE_REPRESENTATION_RELATIONSHIP ( 'NONE' , 'NONE' ,  #11842, #4372 ) ;
#5585 = AXIS2_PLACEMENT_3D ( 'NONE', #2733, #6421, #752 ) ;
#5586 = CARTESIAN_POINT ( 'NONE',  ( 5.000000000000002665, 3.306546357697854226E-16, 2.700000000000000622 ) ) ;
#5587 = DIRECTION ( 'NONE',  ( -1.000000000000000000, 3.469446951953611033E-15, 0.000000000000000000 ) ) ;
#5588 = ORIENTED_EDGE ( 'NONE', *, *, #10184, .T. ) ;
#5589 = CARTESIAN_POINT ( 'NONE',  ( -30.07733313487553772, 77.00000000000709122, 4.660254037819535178 ) ) ;
#5590 = CARTESIAN_POINT ( 'NONE',  ( 0.000000000000000000, 92.00000000000000000, 0.000000000000000000 ) ) ;
#5591 = DIRECTION ( 'NONE',  ( 0.8660254037844348218, -0.5000000000000067724, 0.000000000000000000 ) ) ;
#5592 = DIRECTION ( 'NONE',  ( 1.000000000000000000, 0.000000000000000000, 0.000000000000000000 ) ) ;
#5593 = AXIS2_PLACEMENT_3D ( 'NONE', #5943, #4129, #5824 ) ;
#5594 = AXIS2_PLACEMENT_3D ( 'NONE', #4102, #6911, #9512 ) ;
#5595 = CARTESIAN_POINT ( 'NONE',  ( 8.572527594031474570E-15, -10.00000000000000000, -70.00000000000001421 ) ) ;
#5596 = AXIS2_PLACEMENT_3D ( 'NONE', #9410, #10353, #4438 ) ;
#5597 = EDGE_CURVE ( 'NONE', #5761, #7558, #5237, .T. ) ;
#5598 = EDGE_CURVE ( 'NONE', #3436, #3735, #8087, .T. ) ;
#5599 = ADVANCED_FACE ( 'NONE', ( #7162 ), #3079, .F. ) ;
#5600 = CARTESIAN_POINT ( 'NONE',  ( 8.486113780751869839, 18.52929026929728451, 74.51918556699330054 ) ) ;
#5601 = DIRECTION ( 'NONE',  ( 0.000000000000000000, 0.000000000000000000, -1.000000000000000000 ) ) ;
#5602 = VERTEX_POINT ( 'NONE', #12156 ) ;
#5603 = AXIS2_PLACEMENT_3D ( 'NONE', #4903, #11514, #9807 ) ;
#5604 = AXIS2_PLACEMENT_3D ( 'NONE', #10163, #10348, #10097 ) ;
#5605 = CARTESIAN_POINT ( 'NONE',  ( 8.817456953860944867E-15, 65.00000000000000000, 72.00000000000002842 ) ) ;
#5606 = CARTESIAN_POINT ( 'NONE',  ( 0.000000000000000000, 87.50000000000000000, 0.000000000000000000 ) ) ;
#5607 = DIRECTION ( 'NONE',  ( 0.000000000000000000, 1.000000000000000000, 0.000000000000000000 ) ) ;
#5608 = ORIENTED_EDGE ( 'NONE', *, *, #3387, .T. ) ;
#5609 = CYLINDRICAL_SURFACE ( 'NONE', #5664, 72.00000000000002842 ) ;
#5610 = CARTESIAN_POINT ( 'NONE',  ( 0.000000000000000000, 285.0000000000000568, 0.000000000000000000 ) ) ;
#5611 = CIRCLE ( 'NONE', #3419, 100.0000000000000284 ) ;
#5612 = VERTEX_POINT ( 'NONE', #7475 ) ;
#5613 = CARTESIAN_POINT ( 'NONE',  ( 2.500000000000000000, 2.357898499370431722, -2.818925648462311528E-15 ) ) ;
#5614 = AXIS2_PLACEMENT_3D ( 'NONE', #7370, #2627, #181 ) ;
#5615 = ORIENTED_EDGE ( 'NONE', *, *, #1330, .F. ) ;
#5616 = TOROIDAL_SURFACE ( 'NONE', #7407, 25.00000000000000000, 8.000000000000000000 ) ;
#5617 = DIRECTION ( 'NONE',  ( -0.000000000000000000, -1.000000000000000000, -0.000000000000000000 ) ) ;
#5618 = DIRECTION ( 'NONE',  ( -1.000000000000000000, 0.000000000000000000, 0.000000000000000000 ) ) ;
#5619 = VERTEX_POINT ( 'NONE', #2667 ) ;
#5620 = DIRECTION ( 'NONE',  ( -1.000000000000000000, 0.000000000000000000, -6.938893903907228378E-17 ) ) ;
#5621 = VECTOR ( 'NONE', #1998, 1000.000000000000000 ) ;
#5622 = EDGE_LOOP ( 'NONE', ( #9090, #7420 ) ) ;
#5623 = SHAPE_REPRESENTATION_RELATIONSHIP ( 'NONE' , 'NONE' ,  #778, #6020 ) ;
#5624 = DIRECTION ( 'NONE',  ( 1.000000000000000000, 0.000000000000000000, 6.938893903907229610E-17 ) ) ;
#5625 = DIRECTION ( 'NONE',  ( 0.000000000000000000, 0.000000000000000000, -1.000000000000000000 ) ) ;
#5626 = CARTESIAN_POINT ( 'NONE',  ( -7.474274778359196070, 18.61666975080236597, 80.00000000000000000 ) ) ;
#5627 = ORIENTED_EDGE ( 'NONE', *, *, #12180, .T. ) ;
#5628 = CARTESIAN_POINT ( 'NONE',  ( -1.915364268218909594, 113.1874999986344079, -1.915364268218908927 ) ) ;
#5629 = CARTESIAN_POINT ( 'NONE',  ( 30.00100000000000122, 87.00000000000000000, -8.660254037844435260 ) ) ;
#5630 = AXIS2_PLACEMENT_3D ( 'NONE', #2577, #1526, #11061 ) ;
#5631 = EDGE_CURVE ( 'NONE', #10799, #7703, #1091, .T. ) ;
#5632 = ORIENTED_EDGE ( 'NONE', *, *, #11582, .T. ) ;
#5633 = PLANE ( 'NONE',  #5963 ) ;
#5634 = CARTESIAN_POINT ( 'NONE',  ( 0.000000000000000000, -10.00000000000000000, 0.000000000000000000 ) ) ;
#5635 = ORIENTED_EDGE ( 'NONE', *, *, #4938, .T. ) ;
#5636 = CARTESIAN_POINT ( 'NONE',  ( 21.00000000000000355, 2.516649172247811061E-16, -2.055000000000000160 ) ) ;
#5637 = DIRECTION ( 'NONE',  ( 0.000000000000000000, -0.000000000000000000, 1.000000000000000000 ) ) ;
#5638 = EDGE_LOOP ( 'NONE', ( #11553, #6240, #3700, #10074 ) ) ;
#5639 = CARTESIAN_POINT ( 'NONE',  ( 8.809218870694669690, 29.75000000000019540, 79.50000000000000000 ) ) ;
#5640 = CARTESIAN_POINT ( 'NONE',  ( 10.19254911989241386, 23.71650635094626836, 80.00000000000000000 ) ) ;
#5641 = AXIS2_PLACEMENT_3D ( 'NONE', #4546, #7600, #6361 ) ;
#5642 = CARTESIAN_POINT ( 'NONE',  ( -2.708734124999999882, 111.0624999986344079, 3.317242575922456639E-16 ) ) ;
#5643 = ADVANCED_FACE ( 'NONE', ( #5547 ), #3547, .T. ) ;
#5644 = VERTEX_POINT ( 'NONE', #8395 ) ;
#5645 = ORIENTED_EDGE ( 'NONE', *, *, #6982, .F. ) ;
#5646 = EDGE_CURVE ( 'NONE', #9969, #1793, #4477, .T. ) ;
#5647 = APPLICATION_PROTOCOL_DEFINITION ( 'draft international standard', 'automotive_design', 1998, #557 ) ;
#5648 = AXIS2_PLACEMENT_3D ( 'NONE', #4473, #12092, #3543 ) ;
#5649 = DIRECTION ( 'NONE',  ( 0.000000000000000000, -1.000000000000000000, -0.000000000000000000 ) ) ;
#5650 = PLANE ( 'NONE',  #2160 ) ;
#5651 = ORIENTED_EDGE ( 'NONE', *, *, #2974, .T. ) ;
#5652 = CARTESIAN_POINT ( 'NONE',  ( 69.52686081652184669, 40.00000000000009237, 28.12499999999999645 ) ) ;
#5653 = DIRECTION ( 'NONE',  ( 0.000000000000000000, 0.000000000000000000, 1.000000000000000000 ) ) ;
#5654 = EDGE_CURVE ( 'NONE', #3755, #7589, #2608, .T. ) ;
#5655 = CARTESIAN_POINT ( 'NONE',  ( -10.99915987420040864, 41.36037153982223202, 74.19004793912918672 ) ) ;
#5656 = CARTESIAN_POINT ( 'NONE',  ( 4.025725221640669815, 38.53525403784453118, 79.50000000000000000 ) ) ;
#5657 = AXIS2_PLACEMENT_3D ( 'NONE', #6959, #2222, #6028 ) ;
#5658 = DIRECTION ( 'NONE',  ( 0.7071067811865447972, -0.7071067811865503483, 0.000000000000000000 ) ) ;
#5659 = UNCERTAINTY_MEASURE_WITH_UNIT (LENGTH_MEASURE( 1.000000000000000082E-05 ), #9241, 'distance_accuracy_value', 'NONE');
#5660 = CARTESIAN_POINT ( 'NONE',  ( 71.06140945338827919, 42.80295775297188499, -24.19089746873602209 ) ) ;
#5661 = ORIENTED_EDGE ( 'NONE', *, *, #1611, .T. ) ;
#5662 = LINE ( 'NONE', #11335, #5254 ) ;
#5663 = AXIS2_PLACEMENT_3D ( 'NONE', #11691, #7817, #1093 ) ;
#5664 = AXIS2_PLACEMENT_3D ( 'NONE', #679, #12217, #7292 ) ;
#5665 = ADVANCED_FACE ( 'NONE', ( #9324 ), #10204, .T. ) ;
#5666 = CARTESIAN_POINT ( 'NONE',  ( -5.970153145843347347E-16, 112.7500000000000000, -3.250000000000000444 ) ) ;
#5667 = CARTESIAN_POINT ( 'NONE',  ( 74.18968745904427919, 19.32840679882189860, -24.96588476870653395 ) ) ;
#5668 = VERTEX_POINT ( 'NONE', #8332 ) ;
#5669 = CARTESIAN_POINT ( 'NONE',  ( -3.250000000000001776, 111.5625000000000000, -1.346194077712558279 ) ) ;
#5670 = CARTESIAN_POINT ( 'NONE',  ( 25.00000000000000000, 345.0000000000000568, -59.99999999999999289 ) ) ;
#5671 = VERTEX_POINT ( 'NONE', #4600 ) ;
#5672 = DIRECTION ( 'NONE',  ( 0.000000000000000000, 0.000000000000000000, 1.000000000000000000 ) ) ;
#5673 = AXIS2_PLACEMENT_3D ( 'NONE', #4196, #8982, #9799 ) ;
#5674 = ORIENTED_EDGE ( 'NONE', *, *, #897, .T. ) ;
#5675 = CARTESIAN_POINT ( 'NONE',  ( 6.000000000000000000, 50.00000000000000000, 69.74238309665078361 ) ) ;
#5676 = LINE ( 'NONE', #4487, #3843 ) ;
#5677 = VERTEX_POINT ( 'NONE', #11093 ) ;
#5678 = CARTESIAN_POINT ( 'NONE',  ( 1.990051048614449116E-16, 111.1249999972688158, 3.250000000000000444 ) ) ;
#5679 = DIRECTION ( 'NONE',  ( 0.000000000000000000, 1.000000000000000000, 0.000000000000000000 ) ) ;
#5680 = VERTEX_POINT ( 'NONE', #6478 ) ;
#5681 =( NAMED_UNIT ( * ) PLANE_ANGLE_UNIT ( ) SI_UNIT ( $, .RADIAN. ) );
#5682 = AXIS2_PLACEMENT_3D ( 'NONE', #4731, #4928, #4863 ) ;
#5683 = LINE ( 'NONE', #12293, #1273 ) ;
#5684 = CIRCLE ( 'NONE', #11432, 35.00000000000000000 ) ;
#5685 = CARTESIAN_POINT ( 'NONE',  ( 138.5355339059338462, 63.53553390593273775, 25.00000000000000000 ) ) ;
#5686 = DIRECTION ( 'NONE',  ( 0.000000000000000000, 0.8660254037844380415, -0.5000000000000009992 ) ) ;
#5687 = EDGE_LOOP ( 'NONE', ( #12196, #8467, #7219, #554 ) ) ;
#5688 = CARTESIAN_POINT ( 'NONE',  ( 1.658621287961228566E-16, 110.5624999986344079, 2.708734125000000326 ) ) ;
#5689 = DIRECTION ( 'NONE',  ( 1.000000000000000000, -7.011174048739587977E-15, 0.000000000000000000 ) ) ;
#5690 = MECHANICAL_DESIGN_GEOMETRIC_PRESENTATION_REPRESENTATION (  '', ( #2896 ), #9448 ) ;
#5691 = PRODUCT_DEFINITION_SHAPE ( 'NONE', 'NONE',  #869 ) ;
#5692 = VECTOR ( 'NONE', #4719, 1000.000000000000000 ) ;
#5693 = ORIENTED_EDGE ( 'NONE', *, *, #4907, .F. ) ;
#5694 = DIRECTION ( 'NONE',  ( -1.000000000000000000, 0.000000000000000000, -0.000000000000000000 ) ) ;
#5695 = DIRECTION ( 'NONE',  ( 0.000000000000000000, 1.000000000000000000, 0.000000000000000000 ) ) ;
#5696 = CLOSED_SHELL ( 'NONE', ( #9838, #7689, #8010, #12344, #3651, #6862, #9563, #1558, #8826, #7242, #4236, #4494, #12016, #11381, #10505, #5755, #747, #11597, #3485, #7167, #10541, #683, #1667, #10611, #2830, #2632, #5165, #10739, #12074, #10271, #6602, #6636, #6518, #9491, #4966, #9465, #6760, #7938, #7182, #293, #1607, #224, #9073, #2412, #3227, #6968, #8212, #3991, #4866, #4789, #2915, #11313 ) ) ;
#5697 = ORIENTED_EDGE ( 'NONE', *, *, #5561, .T. ) ;
#5698 = CIRCLE ( 'NONE', #107, 75.00000000000002842 ) ;
#5699 = FACE_OUTER_BOUND ( 'NONE', #2268, .T. ) ;
#5700 = DIRECTION ( 'NONE',  ( -0.4999999999999977796, 0.8660254037844399289, 0.000000000000000000 ) ) ;
#5701 = ORIENTED_EDGE ( 'NONE', *, *, #538, .T. ) ;
#5702 = DIRECTION ( 'NONE',  ( 0.000000000000000000, 0.000000000000000000, 1.000000000000000000 ) ) ;
#5703 = DIRECTION ( 'NONE',  ( 0.000000000000000000, 0.000000000000000000, -1.000000000000000000 ) ) ;
#5704 = ADVANCED_FACE ( 'NONE', ( #10267 ), #5609, .T. ) ;
#5705 = CIRCLE ( 'NONE', #6099, 17.50000000000000000 ) ;
#5706 = CARTESIAN_POINT ( 'NONE',  ( 2.500000000000000000, 1.178949249685212974, -2.042000000000001148 ) ) ;
#5707 = ADVANCED_FACE ( 'NONE', ( #2549 ), #4414, .T. ) ;
#5708 = CARTESIAN_POINT ( 'NONE',  ( 1.121994411437819084, 110.7499999986343937, 2.708734124999999882 ) ) ;
#5709 = ORIENTED_EDGE ( 'NONE', *, *, #7328, .T. ) ;
#5710 = VERTEX_POINT ( 'NONE', #11285 ) ;
#5711 = DIRECTION ( 'NONE',  ( 0.000000000000000000, 0.000000000000000000, 1.000000000000000000 ) ) ;
#5712 = PLANE ( 'NONE',  #2702 ) ;
#5713 = ORIENTED_EDGE ( 'NONE', *, *, #6076, .T. ) ;
#5714 = DIRECTION ( 'NONE',  ( 0.000000000000000000, 0.000000000000000000, 1.000000000000000000 ) ) ;
#5715 = DIRECTION ( 'NONE',  ( 0.000000000000000000, 0.000000000000000000, 1.000000000000000000 ) ) ;
#5716 = AXIS2_PLACEMENT_3D ( 'NONE', #1343, #3266, #6201 ) ;
#5717 = CARTESIAN_POINT ( 'NONE',  ( -31.11163258972580081, 76.09530646335886672, 6.227229208586041231 ) ) ;
#5718 = CARTESIAN_POINT ( 'NONE',  ( 145.0000000000011369, 225.0000000000000853, -20.00000000000000000 ) ) ;
#5719 = EDGE_CURVE ( 'NONE', #10079, #6241, #2775, .T. ) ;
#5720 = EDGE_CURVE ( 'NONE', #11439, #10304, #2277, .T. ) ;
#5721 = CIRCLE ( 'NONE', #7103, 110.0000000000000284 ) ;
#5722 = CARTESIAN_POINT ( 'NONE',  ( 71.99568681135052373, 45.03885011699624386, -21.09760594592234284 ) ) ;
#5723 =( LENGTH_UNIT ( ) NAMED_UNIT ( * ) SI_UNIT ( .MILLI., .METRE. ) );
#5724 = ORIENTED_EDGE ( 'NONE', *, *, #5318, .T. ) ;
#5725 = EDGE_CURVE ( 'NONE', #5612, #6532, #8237, .T. ) ;
#5726 = EDGE_CURVE ( 'NONE', #3399, #11988, #5423, .T. ) ;
#5727 = LINE ( 'NONE', #6651, #12020 ) ;
#5728 = LINE ( 'NONE', #11398, #5692 ) ;
#5729 = CARTESIAN_POINT ( 'NONE',  ( 71.69660397288473064, 15.34952436719795621, -22.14258685050887365 ) ) ;
#5730 = VERTEX_POINT ( 'NONE', #9266 ) ;
#5731 = FACE_OUTER_BOUND ( 'NONE', #7366, .T. ) ;
#5732 = CARTESIAN_POINT ( 'NONE',  ( -1.915364268218909150, 110.6874999986344079, 1.915364268218909594 ) ) ;
#5733 = ORIENTED_EDGE ( 'NONE', *, *, #2906, .T. ) ;
#5734 = CARTESIAN_POINT ( 'NONE',  ( 0.000000000000000000, 65.00000000000000000, 0.000000000000000000 ) ) ;
#5735 = VERTEX_POINT ( 'NONE', #5483 ) ;
#5736 = FACE_OUTER_BOUND ( 'NONE', #2622, .T. ) ;
#5737 = CARTESIAN_POINT ( 'NONE',  ( 0.000000000000000000, -1.178949249685214307, 2.042000000000001592 ) ) ;
#5738 = ORIENTED_EDGE ( 'NONE', *, *, #6955, .F. ) ;
#5739 =( REPRESENTATION_RELATIONSHIP ('NONE','NONE', #3713, #8876 ) REPRESENTATION_RELATIONSHIP_WITH_TRANSFORMATION ( #5301 )SHAPE_REPRESENTATION_RELATIONSHIP( ) );
#5740 = CARTESIAN_POINT ( 'NONE',  ( -2.298097038856279806, 111.4999999972688158, -2.298097038856279362 ) ) ;
#5741 = CARTESIAN_POINT ( 'NONE',  ( 0.000000000000000000, 0.000000000000000000, 79.50000000000000000 ) ) ;
#5742 = ORIENTED_EDGE ( 'NONE', *, *, #4138, .T. ) ;
#5743 =( LENGTH_UNIT ( ) NAMED_UNIT ( * ) SI_UNIT ( .MILLI., .METRE. ) );
#5744 = DIRECTION ( 'NONE',  ( -1.000000000000000000, 0.000000000000000000, -0.000000000000000000 ) ) ;
#5745 = DIRECTION ( 'NONE',  ( 0.000000000000000000, -1.000000000000000000, 0.000000000000000000 ) ) ;
#5746 = LINE ( 'NONE', #6737, #9373 ) ;
#5747 = AXIS2_PLACEMENT_3D ( 'NONE', #8843, #1501, #11918 ) ;
#5748 = PRESENTATION_LAYER_ASSIGNMENT (  '', '', ( #6364 ) ) ;
#5749 = EDGE_LOOP ( 'NONE', ( #2154, #10631, #6381, #11929 ) ) ;
#5750 = CARTESIAN_POINT ( 'NONE',  ( -2.708734124999999882, 112.9999999986343937, 1.121994411437818862 ) ) ;
#5751 = CARTESIAN_POINT ( 'NONE',  ( 3.249999999999999556, 112.8124999972688158, -1.346194077712561610 ) ) ;
#5752 = ADVANCED_FACE ( 'NONE', ( #8208 ), #12031, .T. ) ;
#5753 = VERTEX_POINT ( 'NONE', #12096 ) ;
#5754 = CARTESIAN_POINT ( 'NONE',  ( 11.80921887069467324, 29.75000000000018474, 80.00000000000000000 ) ) ;
#5755 = ADVANCED_FACE ( 'NONE', ( #7351, #1739 ), #4538, .T. ) ;
#5756 = AXIS2_PLACEMENT_3D ( 'NONE', #12292, #4552, #6368 ) ;
#5757 = FACE_OUTER_BOUND ( 'NONE', #3793, .T. ) ;
#5758 = ORIENTED_EDGE ( 'NONE', *, *, #10921, .T. ) ;
#5759 = CARTESIAN_POINT ( 'NONE',  ( 32.15778161310143446, 87.00000000000000000, 8.660254037844435260 ) ) ;
#5760 = LINE ( 'NONE', #4003, #8662 ) ;
#5761 = VERTEX_POINT ( 'NONE', #10640 ) ;
#5762 = DIRECTION ( 'NONE',  ( 0.000000000000000000, 0.000000000000000000, 1.000000000000000000 ) ) ;
#5763 = LINE ( 'NONE', #9542, #7303 ) ;
#5764 = DIRECTION ( 'NONE',  ( -0.8660254037844398178, -0.4999999999999977796, 0.000000000000000000 ) ) ;
#5765 = CARTESIAN_POINT ( 'NONE',  ( -2.708734125000000326, 114.1249999986344079, -1.121994411437818195 ) ) ;
#5766 = CARTESIAN_POINT ( 'NONE',  ( 1.990051048614449116E-16, 112.2500000000000000, 3.250000000000000444 ) ) ;
#5767 = FACE_OUTER_BOUND ( 'NONE', #7957, .T. ) ;
#5768 = ORIENTED_EDGE ( 'NONE', *, *, #9964, .F. ) ;
#5769 = FILL_AREA_STYLE_COLOUR ( '', #8936 ) ;
#5770 = EDGE_LOOP ( 'NONE', ( #9149, #3394, #7807, #8336 ) ) ;
#5771 = CARTESIAN_POINT ( 'NONE',  ( -20.00000000000004263, 54.99999999999999289, 67.08203932499370126 ) ) ;
#5772 = CARTESIAN_POINT ( 'NONE',  ( 0.000000000000000000, 115.0000000000000000, 3.399999999999999911 ) ) ;
#5773 = ORIENTED_EDGE ( 'NONE', *, *, #1022, .F. ) ;
#5774 = CARTESIAN_POINT ( 'NONE',  ( 20.00000000000000355, 63.00000000000000000, 57.08203932499370836 ) ) ;
#5775 = AXIS2_PLACEMENT_3D ( 'NONE', #4190, #7812, #7922 ) ;
#5776 = AXIS2_PLACEMENT_3D ( 'NONE', #1139, #11616, #4000 ) ;
#5777 = DIRECTION ( 'NONE',  ( -0.000000000000000000, 1.000000000000000000, -0.000000000000000000 ) ) ;
#5778 =( BOUNDED_CURVE ( )  B_SPLINE_CURVE ( 3, ( #2698, #4442, #8303, #10297 ),
 .UNSPECIFIED., .F., .F. ) 
 B_SPLINE_CURVE_WITH_KNOTS ( ( 4, 4 ),
 ( 1.860548028230944562, 2.013707370868536461 ),
 .UNSPECIFIED. ) 
 CURVE ( )  GEOMETRIC_REPRESENTATION_ITEM ( )  RATIONAL_B_SPLINE_CURVE ( ( 1.000000000000000000, 0.9980461397859388128, 0.9980461397859388128, 1.000000000000000000 ) ) 
 REPRESENTATION_ITEM ( '' )  );
#5779 = CARTESIAN_POINT ( 'NONE',  ( 0.000000000000000000, 75.00000000000001421, -98.00000000000001421 ) ) ;
#5780 = FACE_OUTER_BOUND ( 'NONE', #3979, .T. ) ;
#5781 = SHAPE_REPRESENTATION_RELATIONSHIP ( 'NONE' , 'NONE' ,  #9674, #10022 ) ;
#5782 = AXIS2_PLACEMENT_3D ( 'NONE', #684, #10272, #1743 ) ;
#5783 = EDGE_CURVE ( 'NONE', #357, #4020, #484, .T. ) ;
#5784 = CARTESIAN_POINT ( 'NONE',  ( 71.26020304811987671, 48.71088408138511738, -23.39373652035234841 ) ) ;
#5785 = CARTESIAN_POINT ( 'NONE',  ( -24.76446302067273209, 275.0000000000000000, -102.0378428393002679 ) ) ;
#5786 = DIRECTION ( 'NONE',  ( 0.000000000000000000, 1.000000000000000000, 0.000000000000000000 ) ) ;
#5787 = CARTESIAN_POINT ( 'NONE',  ( 100.7495955565343451, 275.0000000000000000, 29.57226733266770680 ) ) ;
#5788 = CARTESIAN_POINT ( 'NONE',  ( 75.74050859682202486, 15.90871218390771347, -22.87883167916282900 ) ) ;
#5789 = ORIENTED_EDGE ( 'NONE', *, *, #304, .T. ) ;
#5790 = PLANE ( 'NONE',  #894 ) ;
#5791 = CIRCLE ( 'NONE', #2771, 17.50000000000000000 ) ;
#5792 = FACE_OUTER_BOUND ( 'NONE', #7251, .T. ) ;
#5793 = ORIENTED_EDGE ( 'NONE', *, *, #5654, .F. ) ;
#5794 = FACE_OUTER_BOUND ( 'NONE', #9070, .T. ) ;
#5795 = EDGE_CURVE ( 'NONE', #12197, #5535, #8762, .T. ) ;
#5796 = VECTOR ( 'NONE', #900, 1000.000000000000000 ) ;
#5797 = EDGE_LOOP ( 'NONE', ( #8122, #1171, #2144, #2319 ) ) ;
#5798 = CARTESIAN_POINT ( 'NONE',  ( 10.19254911989230727, 36.28349364905406560, 79.50000000000000000 ) ) ;
#5799 = CARTESIAN_POINT ( 'NONE',  ( 74.75199569173395275, 42.65375252791112359, 24.25052255086779951 ) ) ;
#5800 = EDGE_LOOP ( 'NONE', ( #6656, #5709, #5550, #11223 ) ) ;
#5801 = CARTESIAN_POINT ( 'NONE',  ( 0.000000000000000000, 122.0000000000000000, -17.50000000000000000 ) ) ;
#5802 = DIRECTION ( 'NONE',  ( 0.000000000000000000, 0.000000000000000000, 1.000000000000000000 ) ) ;
#5803 = ORIENTED_EDGE ( 'NONE', *, *, #11643, .T. ) ;
#5804 = DIRECTION ( 'NONE',  ( -0.7071067811865495711, -0.7071067811865455743, -0.000000000000000000 ) ) ;
#5806 = LINE ( 'NONE', #4736, #2424 ) ;
#5805 = AXIS2_PLACEMENT_3D ( 'NONE', #5315, #6124, #11868 ) ;
#5807 = CARTESIAN_POINT ( 'NONE',  ( 0.000000000000000000, 75.00000000000001421, -100.0000000000000142 ) ) ;
#5808 = ORIENTED_EDGE ( 'NONE', *, *, #1551, .T. ) ;
#5809 = CARTESIAN_POINT ( 'NONE',  ( -2.708734125000000770, 113.8749999986343937, -1.121994411437818639 ) ) ;
#5810 = CARTESIAN_POINT ( 'NONE',  ( -5.970153145843347347E-16, 112.6249999972688158, -3.250000000000000444 ) ) ;
#5811 = AXIS2_PLACEMENT_3D ( 'NONE', #5405, #10249, #7458 ) ;
#5812 = AXIS2_PLACEMENT_3D ( 'NONE', #8529, #9525, #5625 ) ;
#5813 = EDGE_LOOP ( 'NONE', ( #7963, #3972, #5914, #4566 ) ) ;
#5814 = FACE_OUTER_BOUND ( 'NONE', #5482, .T. ) ;
#5815 = DIRECTION ( 'NONE',  ( -0.000000000000000000, -1.000000000000000000, -0.000000000000000000 ) ) ;
#5816 = ORIENTED_EDGE ( 'NONE', *, *, #11731, .T. ) ;
#5817 = DIRECTION ( 'NONE',  ( 0.4999999999999985567, 0.8660254037844394848, 0.000000000000000000 ) ) ;
#5818 = CARTESIAN_POINT ( 'NONE',  ( 69.52686081652183248, 19.67220229193595316, 28.12500000000000355 ) ) ;
#5819 = EDGE_LOOP ( 'NONE', ( #5033, #4130, #4981, #11855 ) ) ;
#5820 = DIRECTION ( 'NONE',  ( -0.000000000000000000, -1.000000000000000000, -0.000000000000000000 ) ) ;
#5821 = ADVANCED_FACE ( 'NONE', ( #231, #38 ), #5790, .T. ) ;
#5822 = EDGE_CURVE ( 'NONE', #2754, #1921, #5912, .T. ) ;
#5823 = DIRECTION ( 'NONE',  ( -0.000000000000000000, 1.000000000000000000, -0.000000000000000000 ) ) ;
#5824 = DIRECTION ( 'NONE',  ( 0.000000000000000000, -0.000000000000000000, 1.000000000000000000 ) ) ;
#5825 = CARTESIAN_POINT ( 'NONE',  ( -5.970153145843347347E-16, 114.6249999972688158, -3.250000000000000444 ) ) ;
#5826 = DIRECTION ( 'NONE',  ( -0.000000000000000000, -1.000000000000000000, -0.000000000000000000 ) ) ;
#5827 = CARTESIAN_POINT ( 'NONE',  ( 1.121994411437819084, 114.3749999986344221, -2.708734124999999437 ) ) ;
#5828 = EDGE_CURVE ( 'NONE', #9195, #5986, #7850, .T. ) ;
#5829 = VERTEX_POINT ( 'NONE', #4785 ) ;
#5830 =( LENGTH_UNIT ( ) NAMED_UNIT ( * ) SI_UNIT ( .MILLI., .METRE. ) );
#5831 = ORIENTED_EDGE ( 'NONE', *, *, #4726, .T. ) ;
#5832 = CARTESIAN_POINT ( 'NONE',  ( 165.0000000000011369, 37.07106781186553945, 25.00000000000000000 ) ) ;
#5833 = PLANE ( 'NONE',  #6088 ) ;
#5834 = AXIS2_PLACEMENT_3D ( 'NONE', #1034, #8624, #8498 ) ;
#5835 = ORIENTED_EDGE ( 'NONE', *, *, #2156, .F. ) ;
#5836 = CARTESIAN_POINT ( 'NONE',  ( 75.00000000000001421, 45.00000000000008527, 25.00000000000000000 ) ) ;
#5837 = CARTESIAN_POINT ( 'NONE',  ( -69.85388127645425982, 77.00000000000000000, 8.660254037844445918 ) ) ;
#5838 = CARTESIAN_POINT ( 'NONE',  ( -30.94187416189151918, 76.19472969970551901, 6.055023111780714729 ) ) ;
#5839 = CARTESIAN_POINT ( 'NONE',  ( -1.121994411437820194, 110.9999999986343937, -2.708734124999999882 ) ) ;
#5840 = ORIENTED_EDGE ( 'NONE', *, *, #9998, .T. ) ;
#5841 = VECTOR ( 'NONE', #1362, 1000.000000000000000 ) ;
#5842 = CARTESIAN_POINT ( 'NONE',  ( 70.10024745330821361, 45.37027644699535500, -26.66438925502398760 ) ) ;
#5843 = EDGE_CURVE ( 'NONE', #4721, #3448, #11527, .T. ) ;
#5844 = CARTESIAN_POINT ( 'NONE',  ( 8.809218870694669690, 30.25000000000019540, 79.50000000000000000 ) ) ;
#5845 = LINE ( 'NONE', #161, #1422 ) ;
#5846 = DIRECTION ( 'NONE',  ( 0.000000000000000000, 1.000000000000000000, 0.000000000000000000 ) ) ;
#5847 = CARTESIAN_POINT ( 'NONE',  ( -9.976035167149682081, 25.21650635094616533, 80.00000000000000000 ) ) ;
#5848 = ORIENTED_EDGE ( 'NONE', *, *, #27, .F. ) ;
#5849 = AXIS2_PLACEMENT_3D ( 'NONE', #3914, #5907, #8755 ) ;
#5850 = DIRECTION ( 'NONE',  ( -0.000000000000000000, -0.000000000000000000, 1.000000000000000000 ) ) ;
#5851 = DIRECTION ( 'NONE',  ( -0.000000000000000000, -0.000000000000000000, 1.000000000000000000 ) ) ;
#5852 = EDGE_CURVE ( 'NONE', #4428, #4212, #10433, .T. ) ;
#5853 = EDGE_LOOP ( 'NONE', ( #12325, #5422, #7172, #6266 ) ) ;
#5854 = CARTESIAN_POINT ( 'NONE',  ( 2.500000000000000000, 2.629050547790028946E-15, 2.042000000000000259 ) ) ;
#5855 = VECTOR ( 'NONE', #4018, 1000.000000000000000 ) ;
#5856 = VECTOR ( 'NONE', #1367, 1000.000000000000000 ) ;
#5857 = ORIENTED_EDGE ( 'NONE', *, *, #4576, .T. ) ;
#5858 = CARTESIAN_POINT ( 'NONE',  ( 7.344472908539098732, 24.78349364905406205, 80.00000000000000000 ) ) ;
#5859 = CARTESIAN_POINT ( 'NONE',  ( 76.23530124607874825, 44.53425327553449620, 22.12995508525856891 ) ) ;
#5860 = EDGE_LOOP ( 'NONE', ( #6852, #4924, #5049, #10282 ) ) ;
#5861 = CARTESIAN_POINT ( 'NONE',  ( 32.61619934561887391, 76.99999999999998579, -8.120688671832020589 ) ) ;
#5862 = DIRECTION ( 'NONE',  ( 0.000000000000000000, -1.000000000000000000, 0.000000000000000000 ) ) ;
#5863 = ORIENTED_EDGE ( 'NONE', *, *, #8017, .T. ) ;
#5864 = EDGE_CURVE ( 'NONE', #4364, #80, #11578, .T. ) ;
#5865 = CARTESIAN_POINT ( 'NONE',  ( -1.190781129305471087, 30.00000000000008882, 80.00000000000000000 ) ) ;
#5866 = DIRECTION ( 'NONE',  ( -0.000000000000000000, -1.000000000000000000, -0.000000000000000000 ) ) ;
#5867 = EDGE_CURVE ( 'NONE', #3256, #12241, #12314, .T. ) ;
#5868 = VECTOR ( 'NONE', #10170, 1000.000000000000000 ) ;
#5869 =( BOUNDED_CURVE ( )  B_SPLINE_CURVE ( 3, ( #6937, #12049, #9092, #7309 ),
 .UNSPECIFIED., .F., .T. ) 
 B_SPLINE_CURVE_WITH_KNOTS ( ( 4, 4 ),
 ( 1.143370257677567281, 1.145717000886475656 ),
 .UNSPECIFIED. ) 
 CURVE ( )  GEOMETRIC_REPRESENTATION_ITEM ( )  RATIONAL_B_SPLINE_CURVE ( ( 1.000000000000000000, 0.9999995410664119788, 0.9999995410664119788, 1.000000000000000000 ) ) 
 REPRESENTATION_ITEM ( '' )  );
#5870 = ORIENTED_EDGE ( 'NONE', *, *, #7210, .F. ) ;
#5871 = CARTESIAN_POINT ( 'NONE',  ( 1.658621287961228566E-16, 111.5624999986344079, 2.708734125000000326 ) ) ;
#5872 = VECTOR ( 'NONE', #3175, 1000.000000000000000 ) ;
#5873 = DIRECTION ( 'NONE',  ( -1.000000000000000000, 0.000000000000000000, 0.000000000000000000 ) ) ;
#5874 = EDGE_LOOP ( 'NONE', ( #1533, #7804, #3202, #1767, #9932 ) ) ;
#5875 = DIRECTION ( 'NONE',  ( -0.000000000000000000, 1.000000000000000000, -0.000000000000000000 ) ) ;
#5876 = CARTESIAN_POINT ( 'NONE',  ( -2.075489372555320955, 14.99018364498190969, 74.97835631650174548 ) ) ;
#5877 = VECTOR ( 'NONE', #6730, 1000.000000000000000 ) ;
#5878 = ORIENTED_EDGE ( 'NONE', *, *, #4649, .F. ) ;
#5879 = AXIS2_PLACEMENT_3D ( 'NONE', #9600, #5935, #3187 ) ;
#5880 = CARTESIAN_POINT ( 'NONE',  ( 89.80805993797383735, 275.0000000000000000, 71.82974571984303225 ) ) ;
#5881 = DIRECTION ( 'NONE',  ( -0.8660254037844457020, -0.4999999999999877875, 0.000000000000000000 ) ) ;
#5882 = VERTEX_POINT ( 'NONE', #2921 ) ;
#5883 = EDGE_CURVE ( 'NONE', #9910, #2786, #1922, .T. ) ;
#5884 = ADVANCED_FACE ( 'NONE', ( #4977 ), #5472, .T. ) ;
#5885 = CARTESIAN_POINT ( 'NONE',  ( 0.000000000000000000, 165.0000000000000000, 0.000000000000000000 ) ) ;
#5886 = CARTESIAN_POINT ( 'NONE',  ( 2.571758278209439492E-16, 153.0000000000000000, -2.099999999999998312 ) ) ;
#5887 = DIRECTION ( 'NONE',  ( -1.000000000000000000, 0.000000000000000000, -0.000000000000000000 ) ) ;
#5888 = CARTESIAN_POINT ( 'NONE',  ( 25.00000000000000000, 345.0000000000000568, -29.99999999999998934 ) ) ;
#5889 = CARTESIAN_POINT ( 'NONE',  ( 0.000000000000000000, 0.000000000000000000, -25.00000000000000000 ) ) ;
#5890 = CARTESIAN_POINT ( 'NONE',  ( 2.708734124999999882, 113.5624999986344079, 0.000000000000000000 ) ) ;
#5891 = VECTOR ( 'NONE', #5406, 1000.000000000000000 ) ;
#5892 = ORIENTED_EDGE ( 'NONE', *, *, #2688, .F. ) ;
#5893 = CARTESIAN_POINT ( 'NONE',  ( 9.942549119892305498, 36.71650635094628967, 80.00000000000000000 ) ) ;
#5894 = CARTESIAN_POINT ( 'NONE',  ( 9.450654096908945471E-15, 44.95265997413478942, 75.00000000000001421 ) ) ;
#5895 = ORIENTED_EDGE ( 'NONE', *, *, #11817, .F. ) ;
#5896 = CYLINDRICAL_SURFACE ( 'NONE', #5834, 15.00000000000000000 ) ;
#5897 = CIRCLE ( 'NONE', #7674, 12.99999999999999822 ) ;
#5898 = CARTESIAN_POINT ( 'NONE',  ( 5.524523187418778569, 18.86875173514745896, 80.00000000000000000 ) ) ;
#5899 = FILL_AREA_STYLE ('',( #4962 ) ) ;
#5900 = CARTESIAN_POINT ( 'NONE',  ( 1.915364268218908927, 111.1874999986344079, -1.915364268218909816 ) ) ;
#5901 = VERTEX_POINT ( 'NONE', #166 ) ;
#5902 = AXIS2_PLACEMENT_3D ( 'NONE', #5455, #8305, #1866 ) ;
#5903 = ORIENTED_EDGE ( 'NONE', *, *, #9348, .F. ) ;
#5904 = VERTEX_POINT ( 'NONE', #2789 ) ;
#5905 = EDGE_CURVE ( 'NONE', #980, #2693, #3673, .T. ) ;
#5906 = VECTOR ( 'NONE', #7023, 1000.000000000000000 ) ;
#5907 = DIRECTION ( 'NONE',  ( 0.000000000000000000, 1.000000000000000000, 0.000000000000000000 ) ) ;
#5908 = DIRECTION ( 'NONE',  ( 0.000000000000000000, -0.000000000000000000, 1.000000000000000000 ) ) ;
#5909 = CARTESIAN_POINT ( 'NONE',  ( 2.708734124999999882, 110.4374999986344079, 0.000000000000000000 ) ) ;
#5910 = CARTESIAN_POINT ( 'NONE',  ( 71.95778018440435631, 10.32676784893601862, -21.14640536576783347 ) ) ;
#5911 = ORIENTED_EDGE ( 'NONE', *, *, #6349, .T. ) ;
#5912 = LINE ( 'NONE', #3853, #7463 ) ;
#5913 = DIRECTION ( 'NONE',  ( -0.000000000000000000, -1.000000000000000000, -0.000000000000000000 ) ) ;
#5914 = ORIENTED_EDGE ( 'NONE', *, *, #2691, .T. ) ;
#5915 = FACE_OUTER_BOUND ( 'NONE', #5819, .T. ) ;
#5916 = VECTOR ( 'NONE', #2077, 999.9999999999998863 ) ;
#5917 = ORIENTED_EDGE ( 'NONE', *, *, #11541, .F. ) ;
#5918 = ADVANCED_FACE ( 'NONE', ( #5731 ), #4722, .T. ) ;
#5919 = CARTESIAN_POINT ( 'NONE',  ( -28.20745110743096262, 86.12135132227002998, -11.13838988601301239 ) ) ;
#5920 = LINE ( 'NONE', #9704, #1055 ) ;
#5921 = ORIENTED_EDGE ( 'NONE', *, *, #1456, .F. ) ;
#5922 = ADVANCED_FACE ( 'NONE', ( #10519 ), #1980, .F. ) ;
#5923 = CARTESIAN_POINT ( 'NONE',  ( -1.346194077712560944, 111.1874999972687874, 3.249999999999998668 ) ) ;
#5924 = CARTESIAN_POINT ( 'NONE',  ( 70.71067811865476926, 20.00000000000009237, -25.00000000000000000 ) ) ;
#5925 = VERTEX_POINT ( 'NONE', #5163 ) ;
#5926 = CONTEXT_DEPENDENT_SHAPE_REPRESENTATION ( #12116, #6885 ) ;
#5927 = DIRECTION ( 'NONE',  ( 0.000000000000000000, 1.000000000000000000, 0.000000000000000000 ) ) ;
#5928 = ORIENTED_EDGE ( 'NONE', *, *, #1622, .T. ) ;
#5929 = CARTESIAN_POINT ( 'NONE',  ( 2.708734125000000326, 112.3124999986344079, 0.000000000000000000 ) ) ;
#5930 = FACE_OUTER_BOUND ( 'NONE', #724, .T. ) ;
#5931 = VERTEX_POINT ( 'NONE', #475 ) ;
#5932 = ADVANCED_FACE ( 'NONE', ( #5105 ), #3100, .T. ) ;
#5933 = ADVANCED_FACE ( 'NONE', ( #3160 ), #8634, .T. ) ;
#5934 = FACE_OUTER_BOUND ( 'NONE', #7350, .T. ) ;
#5935 = DIRECTION ( 'NONE',  ( -1.000000000000000000, 0.000000000000000000, 0.000000000000000000 ) ) ;
#5936 = ORIENTED_EDGE ( 'NONE', *, *, #11731, .F. ) ;
#5937 = DIRECTION ( 'NONE',  ( 0.000000000000000000, 0.000000000000000000, 1.000000000000000000 ) ) ;
#5938 = CARTESIAN_POINT ( 'NONE',  ( 69.57537924859245493, 18.37100271180785072, 28.00483409347995689 ) ) ;
#5939 = CIRCLE ( 'NONE', #2344, 15.00000000000000000 ) ;
#5940 = ORIENTED_EDGE ( 'NONE', *, *, #6484, .F. ) ;
#5941 = FACE_BOUND ( 'NONE', #10861, .T. ) ;
#5942 = CARTESIAN_POINT ( 'NONE',  ( 77.12362621866023460, 44.96938750309810473, -20.63427607811778230 ) ) ;
#5943 = CARTESIAN_POINT ( 'NONE',  ( 0.000000000000000000, 285.0000000000000568, 0.000000000000000000 ) ) ;
#5944 = DIRECTION ( 'NONE',  ( -0.000000000000000000, -1.000000000000000000, -0.000000000000000000 ) ) ;
#5945 = DIRECTION ( 'NONE',  ( 1.000000000000000000, 0.000000000000000000, 0.000000000000000000 ) ) ;
#5946 = CARTESIAN_POINT ( 'NONE',  ( -4.975863863883684959E-16, 112.3124999986344079, -2.708734124999999882 ) ) ;
#5947 = CIRCLE ( 'NONE', #4342, 2.041999999999999815 ) ;
#5948 = EDGE_CURVE ( 'NONE', #12197, #11305, #6963, .T. ) ;
#5949 = EDGE_CURVE ( 'NONE', #2323, #2602, #6218, .T. ) ;
#5950 = AXIS2_PLACEMENT_3D ( 'NONE', #2624, #6611, #1752 ) ;
#5951 = VERTEX_POINT ( 'NONE', #539 ) ;
#5952 = VERTEX_POINT ( 'NONE', #5969 ) ;
#5953 = DIRECTION ( 'NONE',  ( 0.000000000000000000, 0.000000000000000000, 1.000000000000000000 ) ) ;
#5954 = CARTESIAN_POINT ( 'NONE',  ( 12.60718874148162705, 35.90182366188934537, 73.93299872726009880 ) ) ;
#5955 = VERTEX_POINT ( 'NONE', #8821 ) ;
#5956 = DIRECTION ( 'NONE',  ( 0.000000000000000000, 0.000000000000000000, 1.000000000000000000 ) ) ;
#5957 = CARTESIAN_POINT ( 'NONE',  ( 1.088204915335219061E-15, 15.04734002586538821, 75.00000000000001421 ) ) ;
#5958 = CARTESIAN_POINT ( 'NONE',  ( -12.32411137850303184, 36.71650635094619730, 80.00000000000000000 ) ) ;
#5959 = FACE_OUTER_BOUND ( 'NONE', #8517, .T. ) ;
#5960 = LINE ( 'NONE', #1163, #4791 ) ;
#5961 = ORIENTED_EDGE ( 'NONE', *, *, #5631, .T. ) ;
#5962 = VECTOR ( 'NONE', #8456, 1000.000000000000000 ) ;
#5963 = AXIS2_PLACEMENT_3D ( 'NONE', #8478, #3451, #645 ) ;
#5964 = DIRECTION ( 'NONE',  ( -1.000000000000000000, 0.000000000000000000, -0.000000000000000000 ) ) ;
#5965 = DIRECTION ( 'NONE',  ( -0.2358520287683112115, 0.000000000000000000, -0.9717889794219070065 ) ) ;
#5966 = CARTESIAN_POINT ( 'NONE',  ( -27.65180490099799115, 87.90152798314358051, -11.49631016393330540 ) ) ;
#5967 = CARTESIAN_POINT ( 'NONE',  ( -25.00000000000000000, 445.0000000000000568, -95.00000000000000000 ) ) ;
#5968 = CARTESIAN_POINT ( 'NONE',  ( 72.61843774138908714, 15.00000000000009237, -18.74999999999999645 ) ) ;
#5969 = CARTESIAN_POINT ( 'NONE',  ( 2.081899558550500280E-15, 115.0000000000000142, 17.00000000000000000 ) ) ;
#5970 = ADVANCED_FACE ( 'NONE', ( #10764 ), #7149, .F. ) ;
#5971 = EDGE_CURVE ( 'NONE', #1174, #3450, #10888, .T. ) ;
#5972 = LINE ( 'NONE', #8516, #11549 ) ;
#5973 = VECTOR ( 'NONE', #7981, 1000.000000000000000 ) ;
#5974 = VERTEX_POINT ( 'NONE', #4220 ) ;
#5975 = DIRECTION ( 'NONE',  ( -0.000000000000000000, -1.000000000000000000, -0.000000000000000000 ) ) ;
#5976 = STYLED_ITEM ( 'NONE', ( #4716 ), #461 ) ;
#5977 = EDGE_CURVE ( 'NONE', #8953, #7634, #10009, .T. ) ;
#5978 = AXIS2_PLACEMENT_3D ( 'NONE', #964, #5944, #4757 ) ;
#5979 = B_SPLINE_CURVE_WITH_KNOTS ( 'NONE', 3,
 ( #5338, #1659, #5464, #8436, #7457, #8314, #12138, #2649, #1538, #6459, #852, #4394, #1778, #1723, #5530, #12201, #9308, #5589 ),
 .UNSPECIFIED., .F., .F.,
 ( 4, 2, 2, 2, 2, 2, 2, 2, 4 ),
 ( 2.823925224926892107E-17, 0.0008221565609605404907, 0.001644313121921052792, 0.002466469682881565310, 0.003288626243842077395, 0.004110782804802590347, 0.004932939365763108937, 0.005755095926723627527, 0.006577252487684147851 ),
 .UNSPECIFIED. ) ;
#5980 = VERTEX_POINT ( 'NONE', #2226 ) ;
#5981 = AXIS2_PLACEMENT_3D ( 'NONE', #1844, #797, #11140 ) ;
#5982 = FACE_OUTER_BOUND ( 'NONE', #10395, .T. ) ;
#5983 = EDGE_LOOP ( 'NONE', ( #9014, #7002, #457, #6390 ) ) ;
#5984 = PLANE ( 'NONE',  #3681 ) ;
#5985 = CARTESIAN_POINT ( 'NONE',  ( 27.97213591028574342, 86.27509468223338729, 11.40681812415363972 ) ) ;
#5986 = VERTEX_POINT ( 'NONE', #2287 ) ;
#5987 = CARTESIAN_POINT ( 'NONE',  ( -8.000000000000000000, 115.0000000000000000, -5.999999999999998224 ) ) ;
#5988 = DIRECTION ( 'NONE',  ( 0.5000000000000066613, 0.8660254037844347108, 0.000000000000000000 ) ) ;
#5989 = VERTEX_POINT ( 'NONE', #1294 ) ;
#5990 = CARTESIAN_POINT ( 'NONE',  ( -2.708734125000000770, 112.8749999986344079, -1.121994411437818639 ) ) ;
#5991 = CARTESIAN_POINT ( 'NONE',  ( 3.250000000000000444, 113.9374999972688158, 1.346194077712559389 ) ) ;
#5992 = AXIS2_PLACEMENT_3D ( 'NONE', #5734, #5975, #11471 ) ;
#5993 = PRODUCT_DEFINITION_SHAPE ( 'NONE', 'NONE',  #12354 ) ;
#5994 = VERTEX_POINT ( 'NONE', #6096 ) ;
#5995 = CARTESIAN_POINT ( 'NONE',  ( -89.80805993797480369, 285.0000000000000568, 71.82974571984181011 ) ) ;
#5996 = FACE_OUTER_BOUND ( 'NONE', #5749, .T. ) ;
#5997 = EDGE_LOOP ( 'NONE', ( #4956, #7781, #10298, #1470 ) ) ;
#5998 = CARTESIAN_POINT ( 'NONE',  ( -100.7495955565347572, 285.0000000000000568, 29.57226733266631769 ) ) ;
#5999 = CARTESIAN_POINT ( 'NONE',  ( 72.45442684796221045, 10.00000000000009415, 19.38521145883884955 ) ) ;
#6000 = AXIS2_PLACEMENT_3D ( 'NONE', #5375, #3506, #4246 ) ;
#6001 = ORIENTED_EDGE ( 'NONE', *, *, #11148, .T. ) ;
#6002 = DIRECTION ( 'NONE',  ( 1.000000000000000000, -1.040834085586083310E-14, 0.000000000000000000 ) ) ;
#6003 = CARTESIAN_POINT ( 'NONE',  ( 76.77549258727734127, 44.85216755992210125, -21.24643021050508196 ) ) ;
#6004 = FACE_OUTER_BOUND ( 'NONE', #6813, .T. ) ;
#6005 = VERTEX_POINT ( 'NONE', #11900 ) ;
#6006 = CARTESIAN_POINT ( 'NONE',  ( -0.9407811293052826818, 17.00240406844413954, 80.00000000000000000 ) ) ;
#6007 = AXIS2_PLACEMENT_3D ( 'NONE', #3619, #10280, #2619 ) ;
#6008 = EDGE_CURVE ( 'NONE', #5411, #1747, #8942, .T. ) ;
#6009 = CARTESIAN_POINT ( 'NONE',  ( -2.708734125000000326, 113.1249999986344079, -1.121994411437818195 ) ) ;
#6010 = VECTOR ( 'NONE', #9318, 1000.000000000000000 ) ;
#6011 = ORIENTED_EDGE ( 'NONE', *, *, #7796, .T. ) ;
#6012 = CARTESIAN_POINT ( 'NONE',  ( 74.16198487095665826, 19.63722065414038553, 25.00000000000000355 ) ) ;
#6013 = ORIENTED_EDGE ( 'NONE', *, *, #6422, .T. ) ;
#6014 = PRODUCT_DEFINITION_CONTEXT ( 'detailed design', #9946, 'design' ) ;
#6015 = CARTESIAN_POINT ( 'NONE',  ( -6.407287480251391720, 21.46474596215567487, 80.00000000000000000 ) ) ;
#6016 = CARTESIAN_POINT ( 'NONE',  ( 0.000000000000000000, 260.0000000000000000, 100.0000000000000284 ) ) ;
#6017 = ORIENTED_EDGE ( 'NONE', *, *, #865, .T. ) ;
#6018 = FACE_OUTER_BOUND ( 'NONE', #11711, .T. ) ;
#6019 = DIRECTION ( 'NONE',  ( -1.000000000000000000, 0.000000000000000000, -0.000000000000000000 ) ) ;
#6020 = ADVANCED_BREP_SHAPE_REPRESENTATION ( '', ( #8859, #1612 ), #6744 ) ;
#6021 = VECTOR ( 'NONE', #10441, 1000.000000000000000 ) ;
#6022 = CARTESIAN_POINT ( 'NONE',  ( 29.48150359603894088, 285.0000000000000568, -121.4736224277384053 ) ) ;
#6023 = DIRECTION ( 'NONE',  ( 0.000000000000000000, 1.000000000000000000, 0.000000000000000000 ) ) ;
#6024 = EDGE_CURVE ( 'NONE', #9442, #7980, #9759, .T. ) ;
#6025 = ADVANCED_FACE ( 'NONE', ( #4336 ), #10946, .F. ) ;
#6026 = VERTEX_POINT ( 'NONE', #2407 ) ;
#6027 = SURFACE_STYLE_USAGE ( .BOTH. , #2220 ) ;
#6028 = DIRECTION ( 'NONE',  ( 0.000000000000000000, 0.000000000000000000, 1.000000000000000000 ) ) ;
#6029 = CARTESIAN_POINT ( 'NONE',  ( -13.00000000000000178, 127.0000000000000000, 7.483314773547879106 ) ) ;
#6030 = CARTESIAN_POINT ( 'NONE',  ( -1.190781129305471087, 30.00000000000008882, 78.00000000000000000 ) ) ;
#6031 = CARTESIAN_POINT ( 'NONE',  ( 107.1104145097471445, 275.0000000000000000, 41.86118851096031079 ) ) ;
#6032 = EDGE_CURVE ( 'NONE', #7410, #9178, #8551, .T. ) ;
#6033 = CARTESIAN_POINT ( 'NONE',  ( 71.75476781871512344, 10.54753387286905664, -21.82544253889692953 ) ) ;
#6034 = CARTESIAN_POINT ( 'NONE',  ( 2.708734125000000326, 113.3749999986344079, 1.121994411437818862 ) ) ;
#6035 = AXIS2_PLACEMENT_3D ( 'NONE', #12165, #5556, #3677 ) ;
#6036 = ORIENTED_EDGE ( 'NONE', *, *, #4290, .F. ) ;
#6037 = CARTESIAN_POINT ( 'NONE',  ( -14.19078112930546887, 30.00000000000008882, 78.00000000000000000 ) ) ;
#6038 = EDGE_CURVE ( 'NONE', #1734, #5730, #1875, .T. ) ;
#6039 = VERTEX_POINT ( 'NONE', #666 ) ;
#6040 = VECTOR ( 'NONE', #11213, 1000.000000000000000 ) ;
#6041 = EDGE_CURVE ( 'NONE', #5925, #3517, #11080, .T. ) ;
#6042 = CARTESIAN_POINT ( 'NONE',  ( 32.13993895771327658, 87.28197645339800204, 8.497454856569966353 ) ) ;
#6043 = VERTEX_POINT ( 'NONE', #10126 ) ;
#6044 = DIRECTION ( 'NONE',  ( 0.000000000000000000, 0.000000000000000000, 1.000000000000000000 ) ) ;
#6045 = CARTESIAN_POINT ( 'NONE',  ( 27.54203853141984126, 86.50063778822033100, 11.90690952824018467 ) ) ;
#6046 = EDGE_LOOP ( 'NONE', ( #3675, #3115, #11546, #5738 ) ) ;
#6047 = DIRECTION ( 'NONE',  ( 1.000000000000000000, -0.000000000000000000, 1.224646799147353207E-16 ) ) ;
#6048 = DIRECTION ( 'NONE',  ( 0.000000000000000000, 0.000000000000000000, 1.000000000000000000 ) ) ;
#6049 = ORIENTED_EDGE ( 'NONE', *, *, #9054, .T. ) ;
#6050 = CARTESIAN_POINT ( 'NONE',  ( -2.708734125000000326, 111.7499999986344079, 1.121994411437818862 ) ) ;
#6051 = VECTOR ( 'NONE', #7394, 1000.000000000000000 ) ;
#6052 = AXIS2_PLACEMENT_3D ( 'NONE', #3806, #10530, #947 ) ;
#6053 = ORIENTED_EDGE ( 'NONE', *, *, #3515, .F. ) ;
#6054 = EDGE_CURVE ( 'NONE', #11751, #4302, #4400, .T. ) ;
#6055 = CARTESIAN_POINT ( 'NONE',  ( 3.592712519748626931, 21.21474596215575659, 79.50000000000000000 ) ) ;
#6056 = CARTESIAN_POINT ( 'NONE',  ( -12.78987254884215652, 20.47477440642036939, 73.90223226960110026 ) ) ;
#6057 = EDGE_LOOP ( 'NONE', ( #9585, #3859, #4324, #4252, #906 ) ) ;
#6058 = DIRECTION ( 'NONE',  ( -0.000000000000000000, -0.000000000000000000, 1.000000000000000000 ) ) ;
#6059 = CARTESIAN_POINT ( 'NONE',  ( 72.61843774138907293, 10.00000000000017586, 18.75000000000000000 ) ) ;
#6060 = VERTEX_POINT ( 'NONE', #8134 ) ;
#6061 = FACE_OUTER_BOUND ( 'NONE', #8480, .T. ) ;
#6062 = VECTOR ( 'NONE', #11910, 1000.000000000000000 ) ;
#6063 = LINE ( 'NONE', #7810, #2403 ) ;
#6064 = ORIENTED_EDGE ( 'NONE', *, *, #7316, .F. ) ;
#6065 = DIRECTION ( 'NONE',  ( 0.8660254037844348218, -0.5000000000000067724, 0.000000000000000000 ) ) ;
#6066 = CARTESIAN_POINT ( 'NONE',  ( 70.79540202493410561, 19.57470310065012953, 24.98706380095428159 ) ) ;
#6067 = AXIS2_PLACEMENT_3D ( 'NONE', #12152, #3544, #4346 ) ;
#6068 = VECTOR ( 'NONE', #9922, 999.9999999999998863 ) ;
#6069 = ORIENTED_EDGE ( 'NONE', *, *, #9192, .T. ) ;
#6070 = CARTESIAN_POINT ( 'NONE',  ( 0.000000000000000000, 345.0000000000000568, -34.99999999999999289 ) ) ;
#6071 = CARTESIAN_POINT ( 'NONE',  ( 74.21645788709501801, 40.83568806828487396, -24.93253696209796644 ) ) ;
#6072 = ORIENTED_EDGE ( 'NONE', *, *, #7704, .F. ) ;
#6073 = DIRECTION ( 'NONE',  ( -1.000000000000000000, 0.000000000000000000, 0.000000000000000000 ) ) ;
#6074 = CARTESIAN_POINT ( 'NONE',  ( 71.00672680945956472, 48.18257563199676952, 24.14780939829461204 ) ) ;
#6075 = VERTEX_POINT ( 'NONE', #6277 ) ;
#6076 = EDGE_CURVE ( 'NONE', #8201, #2754, #8471, .T. ) ;
#6077 = STYLED_ITEM ( 'NONE', ( #9812 ), #589 ) ;
#6078 = CARTESIAN_POINT ( 'NONE',  ( 5.092712519748611832, 18.61666975080242992, 80.00000000000000000 ) ) ;
#6079 = CYLINDRICAL_SURFACE ( 'NONE', #11543, 3.399999999999999911 ) ;
#6080 = ADVANCED_FACE ( 'NONE', ( #7926 ), #1271, .T. ) ;
#6081 = DIRECTION ( 'NONE',  ( -0.000000000000000000, 1.000000000000000000, -0.000000000000000000 ) ) ;
#6082 = AXIS2_PLACEMENT_3D ( 'NONE', #6906, #8999, #1232 ) ;
#6083 = AXIS2_PLACEMENT_3D ( 'NONE', #7243, #10091, #5373 ) ;
#6084 = ORIENTED_EDGE ( 'NONE', *, *, #10004, .T. ) ;
#6085 = ORIENTED_EDGE ( 'NONE', *, *, #154, .F. ) ;
#6086 = ORIENTED_EDGE ( 'NONE', *, *, #7895, .T. ) ;
#6087 = VECTOR ( 'NONE', #3155, 1000.000000000000000 ) ;
#6088 = AXIS2_PLACEMENT_3D ( 'NONE', #4831, #10499, #9615 ) ;
#6089 =( NAMED_UNIT ( * ) SI_UNIT ( $, .STERADIAN. ) SOLID_ANGLE_UNIT ( ) );
#6090 = EDGE_CURVE ( 'NONE', #828, #12197, #10741, .T. ) ;
#6091 = DIRECTION ( 'NONE',  ( -1.000000000000000000, 0.000000000000000000, 0.000000000000000000 ) ) ;
#6092 = DIRECTION ( 'NONE',  ( 0.000000000000000000, 0.000000000000000000, 1.000000000000000000 ) ) ;
#6093 = VECTOR ( 'NONE', #5607, 1000.000000000000000 ) ;
#6094 = FACE_OUTER_BOUND ( 'NONE', #9527, .T. ) ;
#6095 = DIRECTION ( 'NONE',  ( -0.8660254037844363761, 0.5000000000000038858, 0.000000000000000000 ) ) ;
#6096 = CARTESIAN_POINT ( 'NONE',  ( -16.19078112930547064, 30.00000000000008882, 65.00000000000000000 ) ) ;
#6097 = ADVANCED_FACE ( 'NONE', ( #8174 ), #9860, .F. ) ;
#6098 = CARTESIAN_POINT ( 'NONE',  ( 1.915364268218909594, 112.4374999986344079, 1.915364268218909594 ) ) ;
#6099 = AXIS2_PLACEMENT_3D ( 'NONE', #4511, #6383, #5576 ) ;
#6100 = VERTEX_POINT ( 'NONE', #6070 ) ;
#6101 = DIRECTION ( 'NONE',  ( 0.000000000000000000, 1.000000000000000000, 0.000000000000000000 ) ) ;
#6102 = AXIS2_PLACEMENT_3D ( 'NONE', #5284, #8883, #2286 ) ;
#6103 = ADVANCED_FACE ( 'NONE', ( #5261, #1335 ), #4253, .F. ) ;
#6104 = ADVANCED_FACE ( 'NONE', ( #11875 ), #11749, .T. ) ;
#6105 = ORIENTED_EDGE ( 'NONE', *, *, #7536, .T. ) ;
#6106 = CARTESIAN_POINT ( 'NONE',  ( 77.29386075506076281, 45.00000000000009237, 20.32108226578738197 ) ) ;
#6107 = ORIENTED_EDGE ( 'NONE', *, *, #5548, .T. ) ;
#6108 = CARTESIAN_POINT ( 'NONE',  ( 0.000000000000000000, 0.000000000000000000, 79.50000000000000000 ) ) ;
#6109 = DIRECTION ( 'NONE',  ( -0.7071067811865437980, 0.7071067811865513475, 0.000000000000000000 ) ) ;
#6110 = ORIENTED_EDGE ( 'NONE', *, *, #9437, .T. ) ;
#6111 = AXIS2_PLACEMENT_3D ( 'NONE', #6123, #3318, #3249 ) ;
#6112 = CARTESIAN_POINT ( 'NONE',  ( 77.45966692414835109, 15.00000000000008882, -19.99999999999999645 ) ) ;
#6113 = ORIENTED_EDGE ( 'NONE', *, *, #6232, .T. ) ;
#6114 = CARTESIAN_POINT ( 'NONE',  ( 70.26526821373037990, 46.06560101682759978, -26.22825182065055927 ) ) ;
#6115 = ORIENTED_EDGE ( 'NONE', *, *, #5364, .T. ) ;
#6116 = CARTESIAN_POINT ( 'NONE',  ( -30.00100000000000122, 77.00000000000000000, -8.660254037844445918 ) ) ;
#6117 = LINE ( 'NONE', #1863, #8013 ) ;
#6118 = ORIENTED_EDGE ( 'NONE', *, *, #8600, .T. ) ;
#6119 = CYLINDRICAL_SURFACE ( 'NONE', #8777, 15.00000000000000000 ) ;
#6120 = CARTESIAN_POINT ( 'NONE',  ( 0.000000000000000000, 67.00000000000000000, 0.000000000000000000 ) ) ;
#6121 = ORIENTED_EDGE ( 'NONE', *, *, #8553, .T. ) ;
#6122 = DIRECTION ( 'NONE',  ( 0.000000000000000000, 0.000000000000000000, -1.000000000000000000 ) ) ;
#6123 = CARTESIAN_POINT ( 'NONE',  ( -25.00000000000000000, 570.2996408614167194, -59.99999999999999289 ) ) ;
#6124 = DIRECTION ( 'NONE',  ( -0.000000000000000000, -1.000000000000000000, -0.000000000000000000 ) ) ;
#6125 = ORIENTED_EDGE ( 'NONE', *, *, #4159, .T. ) ;
#6126 = DIRECTION ( 'NONE',  ( -0.000000000000000000, -0.000000000000000000, 1.000000000000000000 ) ) ;
#6127 = EDGE_CURVE ( 'NONE', #5052, #9708, #3658, .T. ) ;
#6128 = CARTESIAN_POINT ( 'NONE',  ( 74.52821641976770195, 17.89711956805382442, 24.53929266990205704 ) ) ;
#6129 = ADVANCED_FACE ( 'NONE', ( #4134 ), #10554, .F. ) ;
#6130 = ORIENTED_EDGE ( 'NONE', *, *, #11534, .T. ) ;
#6131 = CARTESIAN_POINT ( 'NONE',  ( 71.95699135611761221, 49.67243019782949887, -21.14906888506497751 ) ) ;
#6132 = CARTESIAN_POINT ( 'NONE',  ( 10.19046713554723560, 36.28229161483199050, 80.00000000000000000 ) ) ;
#6133 = VERTEX_POINT ( 'NONE', #3845 ) ;
#6134 = DIRECTION ( 'NONE',  ( -0.000000000000000000, -1.000000000000000000, -0.000000000000000000 ) ) ;
#6135 = CARTESIAN_POINT ( 'NONE',  ( 70.30108951986187549, 46.17501438243731116, 26.13045860990727931 ) ) ;
#6136 = ORIENTED_EDGE ( 'NONE', *, *, #3756, .F. ) ;
#6137 = CARTESIAN_POINT ( 'NONE',  ( 25.00000000000000000, 345.0000000000000568, -59.99999999999999289 ) ) ;
#6138 = APPLICATION_CONTEXT ( 'automotive_design' ) ;
#6139 = CARTESIAN_POINT ( 'NONE',  ( 7.594472908538985045, 34.78349364905407270, 79.50000000000000000 ) ) ;
#6140 = CARTESIAN_POINT ( 'NONE',  ( 3.592712519748626931, 21.21474596215575659, 80.00000000000000000 ) ) ;
#6141 = CARTESIAN_POINT ( 'NONE',  ( 2.708734124999999882, 114.2499999986344079, -1.121994411437820416 ) ) ;
#6142 =( GEOMETRIC_REPRESENTATION_CONTEXT ( 3 ) GLOBAL_UNCERTAINTY_ASSIGNED_CONTEXT ( ( #4775 ) ) GLOBAL_UNIT_ASSIGNED_CONTEXT ( ( #10936, #9056, #7199 ) ) REPRESENTATION_CONTEXT ( 'NONE', 'WORKASPACE' ) );
#6143 = EDGE_LOOP ( 'NONE', ( #3324, #12035, #11210, #2971 ) ) ;
#6144 =( NAMED_UNIT ( * ) PLANE_ANGLE_UNIT ( ) SI_UNIT ( $, .RADIAN. ) );
#6145 = ORIENTED_EDGE ( 'NONE', *, *, #9887, .F. ) ;
#6146 = CARTESIAN_POINT ( 'NONE',  ( 0.000000000000000000, 50.00000000000000000, 0.000000000000000000 ) ) ;
#6147 = CARTESIAN_POINT ( 'NONE',  ( -28.48065962374905169, 85.97961707684488886, -10.89289897176423061 ) ) ;
#6148 = CARTESIAN_POINT ( 'NONE',  ( 29.75437749274565391, 83.76094350395922561, 7.050043618115805266 ) ) ;
#6149 = LINE ( 'NONE', #9938, #9576 ) ;
#6150 = DIRECTION ( 'NONE',  ( -0.000000000000000000, -0.000000000000000000, 1.000000000000000000 ) ) ;
#6151 = DIRECTION ( 'NONE',  ( -1.000000000000000000, -0.000000000000000000, -0.000000000000000000 ) ) ;
#6152 = CARTESIAN_POINT ( 'NONE',  ( 72.02249449389087488, 10.26717901559811175, -20.92514131019472146 ) ) ;
#6153 = CARTESIAN_POINT ( 'NONE',  ( 1.915364268218909594, 113.4374999986344079, 1.915364268218909594 ) ) ;
#6154 = EDGE_LOOP ( 'NONE', ( #10020, #1241, #431, #9354 ) ) ;
#6155 = LINE ( 'NONE', #9068, #8164 ) ;
#6156 = ADVANCED_FACE ( 'NONE', ( #11458 ), #11935, .T. ) ;
#6157 = CIRCLE ( 'NONE', #4360, 10.00000000000000888 ) ;
#6158 = ORIENTED_EDGE ( 'NONE', *, *, #4179, .T. ) ;
#6159 = CARTESIAN_POINT ( 'NONE',  ( 97.61745645431939522, 275.0000000000000000, 78.07581056504676553 ) ) ;
#6160 = ORIENTED_EDGE ( 'NONE', *, *, #9074, .T. ) ;
#6161 = DIRECTION ( 'NONE',  ( 0.000000000000000000, -0.000000000000000000, 1.000000000000000000 ) ) ;
#6162 = CARTESIAN_POINT ( 'NONE',  ( 3.250000000000000444, 113.8749999972688158, 0.000000000000000000 ) ) ;
#6163 = ORIENTED_EDGE ( 'NONE', *, *, #11690, .F. ) ;
#6164 = VECTOR ( 'NONE', #9079, 1000.000000000000000 ) ;
#6165 = CARTESIAN_POINT ( 'NONE',  ( 1.102182119232618227E-14, 75.00000000000001421, -90.00000000000002842 ) ) ;
#6166 = ADVANCED_BREP_SHAPE_REPRESENTATION ( '', ( #543, #1612 ), #9911 ) ;
#6167 = DIRECTION ( 'NONE',  ( 0.000000000000000000, -0.000000000000000000, 1.000000000000000000 ) ) ;
#6168 = EDGE_CURVE ( 'NONE', #12189, #6826, #9837, .T. ) ;
#6169 = EDGE_CURVE ( 'NONE', #6660, #8670, #4677, .T. ) ;
#6170 = ORIENTED_EDGE ( 'NONE', *, *, #9305, .F. ) ;
#6171 = CARTESIAN_POINT ( 'NONE',  ( 0.000000000000000000, 265.0000000000000000, -100.0000000000000142 ) ) ;
#6172 = AXIS2_PLACEMENT_3D ( 'NONE', #7964, #10083, #8213 ) ;
#6173 = ORIENTED_EDGE ( 'NONE', *, *, #8858, .F. ) ;
#6174 = ORIENTED_EDGE ( 'NONE', *, *, #749, .T. ) ;
#6175 = DIRECTION ( 'NONE',  ( -1.000000000000000000, 4.163336342344333082E-15, 0.000000000000000000 ) ) ;
#6176 = DIRECTION ( 'NONE',  ( -0.000000000000000000, -1.000000000000000000, -0.000000000000000000 ) ) ;
#6177 = ORIENTED_EDGE ( 'NONE', *, *, #7726, .T. ) ;
#6178 = LINE ( 'NONE', #2370, #22 ) ;
#6179 = DIRECTION ( 'NONE',  ( 0.000000000000000000, -0.000000000000000000, 1.000000000000000000 ) ) ;
#6180 = EDGE_LOOP ( 'NONE', ( #3362, #6427, #3598, #4237 ) ) ;
#6181 = DIRECTION ( 'NONE',  ( 1.000000000000000000, 0.000000000000000000, 0.000000000000000000 ) ) ;
#6182 = DIRECTION ( 'NONE',  ( -0.5000000000000012212, 0.000000000000000000, -0.8660254037844379305 ) ) ;
#6183 = LINE ( 'NONE', #8163, #2612 ) ;
#6184 = CIRCLE ( 'NONE', #9758, 3.399999999999999911 ) ;
#6185 = VERTEX_POINT ( 'NONE', #2572 ) ;
#6186 = CARTESIAN_POINT ( 'NONE',  ( 1.121994411437818862, 110.7499999986343937, 2.708734124999999882 ) ) ;
#6187 = CIRCLE ( 'NONE', #3967, 9.999999999999998224 ) ;
#6188 = CARTESIAN_POINT ( 'NONE',  ( 70.67517779188629845, 12.63729133232783219, 25.10124566575549565 ) ) ;
#6189 = CIRCLE ( 'NONE', #7, 125.0000000000000568 ) ;
#6190 = VERTEX_POINT ( 'NONE', #517 ) ;
#6191 = CARTESIAN_POINT ( 'NONE',  ( 74.31677170407374433, 18.58020549109977892, 24.80746953044373626 ) ) ;
#6192 = DIRECTION ( 'NONE',  ( 1.000000000000000000, -1.387778780781445676E-14, 0.000000000000000000 ) ) ;
#6193 = ORIENTED_EDGE ( 'NONE', *, *, #6398, .T. ) ;
#6194 = ADVANCED_FACE ( 'NONE', ( #3390 ), #9043, .T. ) ;
#6195 = DIRECTION ( 'NONE',  ( 0.000000000000000000, 1.000000000000000000, 0.000000000000000000 ) ) ;
#6196 = EDGE_CURVE ( 'NONE', #5619, #8739, #285, .T. ) ;
#6197 = CARTESIAN_POINT ( 'NONE',  ( 70.93313137955965431, 42.06848318385853247, 24.57887570927810472 ) ) ;
#6198 = VERTEX_POINT ( 'NONE', #6132 ) ;
#6199 = DIRECTION ( 'NONE',  ( 0.000000000000000000, -0.000000000000000000, 1.000000000000000000 ) ) ;
#6200 = DIRECTION ( 'NONE',  ( 0.000000000000000000, -0.000000000000000000, 1.000000000000000000 ) ) ;
#6201 = DIRECTION ( 'NONE',  ( 0.000000000000000000, 0.000000000000000000, 1.000000000000000000 ) ) ;
#6202 = CARTESIAN_POINT ( 'NONE',  ( 1.346194077712585591, 114.6874999972688158, -3.249999999999974687 ) ) ;
#6203 = EDGE_CURVE ( 'NONE', #6185, #5602, #9986, .T. ) ;
#6204 = VECTOR ( 'NONE', #11928, 999.9999999999998863 ) ;
#6205 = VERTEX_POINT ( 'NONE', #646 ) ;
#6206 = ORIENTED_EDGE ( 'NONE', *, *, #9732, .T. ) ;
#6207 = SHAPE_REPRESENTATION_RELATIONSHIP ( 'NONE' , 'NONE' ,  #3316, #8978 ) ;
#6208 = ORIENTED_EDGE ( 'NONE', *, *, #6710, .F. ) ;
#6209 = AXIS2_PLACEMENT_3D ( 'NONE', #11705, #1351, #284 ) ;
#6210 = CARTESIAN_POINT ( 'NONE',  ( 117.9289321881355193, 40.00000000000009237, 25.00000000000000000 ) ) ;
#6211 = CIRCLE ( 'NONE', #234, 65.00000000000001421 ) ;
#6212 = CYLINDRICAL_SURFACE ( 'NONE', #4954, 25.00000000000000000 ) ;
#6213 = CARTESIAN_POINT ( 'NONE',  ( 1.836970198721029589E-15, 115.0000000000000000, 15.00000000000000000 ) ) ;
#6214 = CARTESIAN_POINT ( 'NONE',  ( 11.80921887069467324, 30.25000000000018474, 80.00000000000000000 ) ) ;
#6215 = LINE ( 'NONE', #4459, #12262 ) ;
#6216 = DIRECTION ( 'NONE',  ( 0.000000000000000000, -0.4999999999999976685, 0.8660254037844399289 ) ) ;
#6217 = DIRECTION ( 'NONE',  ( 0.000000000000000000, 1.000000000000000000, 0.000000000000000000 ) ) ;
#6218 = LINE ( 'NONE', #4282, #8829 ) ;
#6219 = CARTESIAN_POINT ( 'NONE',  ( -1.121994411437818862, 112.6249999986343937, 2.708734125000000326 ) ) ;
#6220 = CARTESIAN_POINT ( 'NONE',  ( -20.00000000000000355, 54.99999999999999289, 57.08203932499370836 ) ) ;
#6221 = CARTESIAN_POINT ( 'NONE',  ( 5.200000000000002842, 0.000000000000000000, 0.000000000000000000 ) ) ;
#6222 = VECTOR ( 'NONE', #9991, 1000.000000000000000 ) ;
#6223 = ORIENTED_EDGE ( 'NONE', *, *, #6888, .F. ) ;
#6224 = CARTESIAN_POINT ( 'NONE',  ( 77.45966692414835109, 45.00000000000008527, 20.00000000000000000 ) ) ;
#6225 = ORIENTED_EDGE ( 'NONE', *, *, #1022, .T. ) ;
#6226 = CARTESIAN_POINT ( 'NONE',  ( 77.45966692414835109, 45.00000000000008527, 20.00000000000000000 ) ) ;
#6227 = CARTESIAN_POINT ( 'NONE',  ( 74.40419232661420779, 18.25469906876584147, -24.69784343973813989 ) ) ;
#6228 = ORIENTED_EDGE ( 'NONE', *, *, #2875, .T. ) ;
#6229 = AXIS2_PLACEMENT_3D ( 'NONE', #3310, #9148, #7048 ) ;
#6230 = ADVANCED_FACE ( 'NONE', ( #2382 ), #2452, .F. ) ;
#6231 = DIRECTION ( 'NONE',  ( 0.000000000000000000, 1.000000000000000000, 0.000000000000000000 ) ) ;
#6232 = EDGE_CURVE ( 'NONE', #11371, #7950, #6257, .T. ) ;
#6233 = CARTESIAN_POINT ( 'NONE',  ( 4.999999999999997335, 0.000000000000000000, 0.000000000000000000 ) ) ;
#6234 = ORIENTED_EDGE ( 'NONE', *, *, #10993, .T. ) ;
#6235 = CARTESIAN_POINT ( 'NONE',  ( 69.52686081652183248, 40.32779770806423159, -28.12499999999998934 ) ) ;
#6236 = VECTOR ( 'NONE', #2367, 1000.000000000000000 ) ;
#6237 = ORIENTED_EDGE ( 'NONE', *, *, #7617, .T. ) ;
#6238 = DIRECTION ( 'NONE',  ( 0.000000000000000000, 0.000000000000000000, 1.000000000000000000 ) ) ;
#6239 = CARTESIAN_POINT ( 'NONE',  ( 0.000000000000000000, 153.0000000000000000, 0.000000000000000000 ) ) ;
#6240 = ORIENTED_EDGE ( 'NONE', *, *, #2349, .F. ) ;
#6241 = VERTEX_POINT ( 'NONE', #8110 ) ;
#6242 = CARTESIAN_POINT ( 'NONE',  ( 1.224646799147353375E-14, 75.00000000000001421, 100.0000000000000142 ) ) ;
#6243 = DIRECTION ( 'NONE',  ( 0.000000000000000000, 1.000000000000000000, 0.000000000000000000 ) ) ;
#6244 = ORIENTED_EDGE ( 'NONE', *, *, #435, .F. ) ;
#6245 = ADVANCED_FACE ( 'NONE', ( #8984 ), #7188, .T. ) ;
#6246 = CARTESIAN_POINT ( 'NONE',  ( 77.45966692414835109, 15.00000000000008882, 20.00000000000000000 ) ) ;
#6247 = FACE_OUTER_BOUND ( 'NONE', #6487, .T. ) ;
#6248 = DIRECTION ( 'NONE',  ( 0.000000000000000000, 0.000000000000000000, -1.000000000000000000 ) ) ;
#6249 = VECTOR ( 'NONE', #9320, 1000.000000000000227 ) ;
#6250 = EDGE_LOOP ( 'NONE', ( #3047, #9900, #12026, #6867 ) ) ;
#6251 = CARTESIAN_POINT ( 'NONE',  ( 3.250000000000000444, 112.0000000000000000, 0.000000000000000000 ) ) ;
#6252 = CARTESIAN_POINT ( 'NONE',  ( 74.37657609242243950, 18.35338373004630341, 24.73263046052399972 ) ) ;
#6253 = ORIENTED_EDGE ( 'NONE', *, *, #7802, .F. ) ;
#6254 = EDGE_CURVE ( 'NONE', #4965, #10014, #452, .T. ) ;
#6255 = CARTESIAN_POINT ( 'NONE',  ( 76.59657895567488595, 15.23512201424183843, 21.54700147973310820 ) ) ;
#6256 = EDGE_CURVE ( 'NONE', #2693, #980, #12257, .T. ) ;
#6257 = LINE ( 'NONE', #7126, #6068 ) ;
#6258 = VECTOR ( 'NONE', #4200, 1000.000000000000000 ) ;
#6259 = ORIENTED_EDGE ( 'NONE', *, *, #1454, .F. ) ;
#6260 = CARTESIAN_POINT ( 'NONE',  ( -5.970153145843347347E-16, 110.7500000000000000, -3.250000000000000444 ) ) ;
#6261 = CARTESIAN_POINT ( 'NONE',  ( 70.03362437693273534, 45.09447798584402989, 26.84082993662288175 ) ) ;
#6262 = ORIENTED_EDGE ( 'NONE', *, *, #9673, .F. ) ;
#6263 = CARTESIAN_POINT ( 'NONE',  ( 1.121994411437819084, 111.4999999986343937, 2.708734125000000326 ) ) ;
#6264 = ORIENTED_EDGE ( 'NONE', *, *, #8272, .T. ) ;
#6265 = AXIS2_PLACEMENT_3D ( 'NONE', #6657, #6780, #7716 ) ;
#6266 = ORIENTED_EDGE ( 'NONE', *, *, #8397, .F. ) ;
#6267 = EDGE_CURVE ( 'NONE', #9708, #6555, #5478, .T. ) ;
#6268 = UNCERTAINTY_MEASURE_WITH_UNIT (LENGTH_MEASURE( 1.000000000000000082E-05 ), #10444, 'distance_accuracy_value', 'NONE');
#6269 = DIRECTION ( 'NONE',  ( -0.000000000000000000, -0.000000000000000000, 1.000000000000000000 ) ) ;
#6270 = CARTESIAN_POINT ( 'NONE',  ( 1.990051048614449116E-16, 111.2500000000000000, 3.250000000000000444 ) ) ;
#6271 = LINE ( 'NONE', #1229, #4059 ) ;
#6272 = AXIS2_PLACEMENT_3D ( 'NONE', #5606, #6348, #1736 ) ;
#6273 = CARTESIAN_POINT ( 'NONE',  ( 0.000000000000000000, 260.0000000000000000, -100.0000000000000142 ) ) ;
#6274 = CARTESIAN_POINT ( 'NONE',  ( -27.53586651884020498, 87.45908356336337874, -11.91741659355894889 ) ) ;
#6275 = CARTESIAN_POINT ( 'NONE',  ( -1.440781129305261477, 20.00000000000009592, 80.00000000000000000 ) ) ;
#6276 = CARTESIAN_POINT ( 'NONE',  ( -1.190781129305471087, 43.00000000000008527, 80.00000000000000000 ) ) ;
#6277 = CARTESIAN_POINT ( 'NONE',  ( -7.474274778359196070, 18.61666975080236597, 79.50000000000000000 ) ) ;
#6278 = CARTESIAN_POINT ( 'NONE',  ( 1.346194077712559389, 110.1875000000000142, 3.250000000000000444 ) ) ;
#6279 = PRESENTATION_LAYER_ASSIGNMENT (  '', '', ( #6077 ) ) ;
#6280 = COLOUR_RGB ( '', 0.31764706, 0.68627451, 0.89019608) ;
#6281 = CARTESIAN_POINT ( 'NONE',  ( -1.440781129305471087, 40.00000000000008527, 79.50000000000000000 ) ) ;
#6282 = CARTESIAN_POINT ( 'NONE',  ( -5.970153145843347347E-16, 113.7500000000000000, -3.250000000000000444 ) ) ;
#6283 = ADVANCED_FACE ( 'NONE', ( #9165 ), #12058, .T. ) ;
#6284 = CIRCLE ( 'NONE', #4480, 14.99999999999999822 ) ;
#6285 = CARTESIAN_POINT ( 'NONE',  ( 74.16198487095665826, 20.00000000000009237, 25.00000000000000000 ) ) ;
#6286 = ORIENTED_EDGE ( 'NONE', *, *, #854, .F. ) ;
#6287 = CARTESIAN_POINT ( 'NONE',  ( 31.88521078284830423, 84.50000000000000000, 10.10362971081847228 ) ) ;
#6288 = ORIENTED_EDGE ( 'NONE', *, *, #671, .F. ) ;
#6289 = FACE_OUTER_BOUND ( 'NONE', #5174, .T. ) ;
#6290 = CARTESIAN_POINT ( 'NONE',  ( 76.59271415824169082, 15.23730819188808283, -21.55336028430495787 ) ) ;
#6291 = ORIENTED_EDGE ( 'NONE', *, *, #11796, .F. ) ;
#6292 = VECTOR ( 'NONE', #1143, 1000.000000000000114 ) ;
#6293 = DIRECTION ( 'NONE',  ( -0.000000000000000000, -0.000000000000000000, 1.000000000000000000 ) ) ;
#6294 = CARTESIAN_POINT ( 'NONE',  ( 2.500000000000000000, -2.357898499370432166, 3.035766082959412415E-15 ) ) ;
#6295 = ORIENTED_EDGE ( 'NONE', *, *, #1138, .T. ) ;
#6296 = CARTESIAN_POINT ( 'NONE',  ( 69.52686081652184669, 40.00000000000009237, -28.12499999999999645 ) ) ;
#6297 = AXIS2_PLACEMENT_3D ( 'NONE', #6918, #300, #3866 ) ;
#6298 = EDGE_CURVE ( 'NONE', #7972, #5022, #6380, .T. ) ;
#6299 = EDGE_CURVE ( 'NONE', #3797, #7113, #7857, .T. ) ;
#6300 = ORIENTED_EDGE ( 'NONE', *, *, #11024, .T. ) ;
#6301 = CARTESIAN_POINT ( 'NONE',  ( 10.19046713554732619, 23.71770838516835411, 80.00000000000000000 ) ) ;
#6302 = ORIENTED_EDGE ( 'NONE', *, *, #10384, .F. ) ;
#6303 = VECTOR ( 'NONE', #6764, 1000.000000000000000 ) ;
#6304 = LINE ( 'NONE', #10088, #8183 ) ;
#6305 = CARTESIAN_POINT ( 'NONE',  ( -30.08147999331295352, 76.80445198238156479, 4.520396356853239261 ) ) ;
#6306 = ORIENTED_EDGE ( 'NONE', *, *, #1256, .F. ) ;
#6307 = CARTESIAN_POINT ( 'NONE',  ( 0.000000000000000000, 335.0000000000000000, 0.000000000000000000 ) ) ;
#6308 = DIRECTION ( 'NONE',  ( 0.000000000000000000, -0.8660254037844402619, 0.4999999999999975575 ) ) ;
#6309 = CARTESIAN_POINT ( 'NONE',  ( 5.525725221640672480, 41.13333024919784719, 79.50000000000000000 ) ) ;
#6310 = EDGE_CURVE ( 'NONE', #737, #9831, #9226, .T. ) ;
#6311 = ORIENTED_EDGE ( 'NONE', *, *, #1972, .T. ) ;
#6312 = DIRECTION ( 'NONE',  ( 0.000000000000000000, 1.000000000000000000, 0.000000000000000000 ) ) ;
#6313 = CARTESIAN_POINT ( 'NONE',  ( 27.33018067101282966, 87.00000000000000000, 12.37179148263486539 ) ) ;
#6314 = VECTOR ( 'NONE', #7744, 1000.000000000000000 ) ;
#6315 = EDGE_CURVE ( 'NONE', #8, #8579, #11815, .T. ) ;
#6316 = EDGE_CURVE ( 'NONE', #3643, #7067, #7379, .T. ) ;
#6317 = EDGE_LOOP ( 'NONE', ( #1691, #11689, #9763, #650 ) ) ;
#6318 = DIRECTION ( 'NONE',  ( 1.000000000000000000, 0.000000000000000000, -0.000000000000000000 ) ) ;
#6319 = CARTESIAN_POINT ( 'NONE',  ( 0.000000000000000000, 122.5000000000000000, 0.000000000000000000 ) ) ;
#6320 = ORIENTED_EDGE ( 'NONE', *, *, #11812, .T. ) ;
#6321 = CARTESIAN_POINT ( 'NONE',  ( 70.88237045016090576, 41.67245225087944505, 24.73035864412370799 ) ) ;
#6322 = ORIENTED_EDGE ( 'NONE', *, *, #4621, .F. ) ;
#6323 = DIRECTION ( 'NONE',  ( 1.000000000000000000, 0.000000000000000000, 0.000000000000000000 ) ) ;
#6324 = CARTESIAN_POINT ( 'NONE',  ( -97.61745645432043261, 275.0000000000000000, 78.07581056504542971 ) ) ;
#6325 = CARTESIAN_POINT ( 'NONE',  ( -1.121994411437819084, 112.6249999986343937, 2.708734125000000326 ) ) ;
#6326 = CARTESIAN_POINT ( 'NONE',  ( -2.708734125000000326, 113.1249999986343937, -1.121994411437818195 ) ) ;
#6327 = EDGE_CURVE ( 'NONE', #10619, #7679, #2908, .T. ) ;
#6328 = EDGE_LOOP ( 'NONE', ( #4557, #1346, #6822, #4309 ) ) ;
#6329 = ORIENTED_EDGE ( 'NONE', *, *, #8074, .F. ) ;
#6330 = LINE ( 'NONE', #3406, #9726 ) ;
#6331 = CARTESIAN_POINT ( 'NONE',  ( 0.000000000000000000, 275.0000000000000000, 0.000000000000000000 ) ) ;
#6332 = DIRECTION ( 'NONE',  ( 0.000000000000000000, 1.000000000000000000, 0.000000000000000000 ) ) ;
#6333 = ADVANCED_FACE ( 'NONE', ( #5757 ), #6686, .T. ) ;
#6334 = DIRECTION ( 'NONE',  ( 0.000000000000000000, 0.000000000000000000, -1.000000000000000000 ) ) ;
#6335 = CARTESIAN_POINT ( 'NONE',  ( -27.30089691780743877, 86.86968904112121947, -12.43627868308088935 ) ) ;
#6336 = CARTESIAN_POINT ( 'NONE',  ( -25.00000000000000000, 347.0000000000000568, -31.99999999999999289 ) ) ;
#6337 = CIRCLE ( 'NONE', #152, 100.0000000000000284 ) ;
#6338 = CARTESIAN_POINT ( 'NONE',  ( 1.836970198721029589E-15, 265.0000000000000000, 15.00000000000000000 ) ) ;
#6339 =( BOUNDED_CURVE ( )  B_SPLINE_CURVE ( 3, ( #7794, #11611, #3060, #7165 ),
 .UNSPECIFIED., .F., .F. ) 
 B_SPLINE_CURVE_WITH_KNOTS ( ( 4, 4 ),
 ( 0.000000000000000000, 1.570796326794895448 ),
 .UNSPECIFIED. ) 
 CURVE ( )  GEOMETRIC_REPRESENTATION_ITEM ( )  RATIONAL_B_SPLINE_CURVE ( ( 1.000000000000000000, 0.8047378541243652705, 0.8047378541243652705, 1.000000000000000000 ) ) 
 REPRESENTATION_ITEM ( '' )  );
#6340 = CARTESIAN_POINT ( 'NONE',  ( 1.346194077712564940, 111.6874999972687732, -3.249999999999993783 ) ) ;
#6341 = CARTESIAN_POINT ( 'NONE',  ( 2.298097038856279806, 113.1250000000000000, 2.298097038856279806 ) ) ;
#6342 = DIRECTION ( 'NONE',  ( 0.000000000000000000, 0.000000000000000000, -1.000000000000000000 ) ) ;
#6343 = CIRCLE ( 'NONE', #10058, 2.500000000000000444 ) ;
#6344 = CARTESIAN_POINT ( 'NONE',  ( -5.970153145843347347E-16, 112.6249999972688158, -3.250000000000000444 ) ) ;
#6345 = ORIENTED_EDGE ( 'NONE', *, *, #3357, .F. ) ;
#6346 = CARTESIAN_POINT ( 'NONE',  ( 0.000000000000000000, 265.0000000000000000, 0.000000000000000000 ) ) ;
#6347 = EDGE_CURVE ( 'NONE', #9573, #6198, #3882, .T. ) ;
#6348 = DIRECTION ( 'NONE',  ( 0.000000000000000000, 1.000000000000000000, 0.000000000000000000 ) ) ;
#6349 = EDGE_CURVE ( 'NONE', #3517, #6916, #9440, .T. ) ;
#6350 = CARTESIAN_POINT ( 'NONE',  ( 74.19368986856427739, 19.28333586514525777, -24.96097029013992241 ) ) ;
#6351 = VERTEX_POINT ( 'NONE', #10484 ) ;
#6352 = CARTESIAN_POINT ( 'NONE',  ( 27.46866764507870684, 86.65804127256188849, 12.06796414783009297 ) ) ;
#6353 = DIRECTION ( 'NONE',  ( 1.000000000000000000, -6.938893903907222067E-15, 0.000000000000000000 ) ) ;
#6354 = ADVANCED_FACE ( 'NONE', ( #3751 ), #10043, .F. ) ;
#6355 = EDGE_LOOP ( 'NONE', ( #7120, #11247, #417, #2096 ) ) ;
#6356 = DIRECTION ( 'NONE',  ( 0.000000000000000000, 1.000000000000000000, 0.000000000000000000 ) ) ;
#6357 = EDGE_LOOP ( 'NONE', ( #11590, #11028 ) ) ;
#6358 = ORIENTED_EDGE ( 'NONE', *, *, #6627, .F. ) ;
#6359 = CARTESIAN_POINT ( 'NONE',  ( 0.000000000000000000, 109.0000000000000000, 3.399999999999999911 ) ) ;
#6360 = AXIS2_PLACEMENT_3D ( 'NONE', #11287, #8333, #4539 ) ;
#6361 = DIRECTION ( 'NONE',  ( 0.000000000000000000, 0.000000000000000000, -1.000000000000000000 ) ) ;
#6362 = EDGE_LOOP ( 'NONE', ( #6970, #11839, #2811, #1777 ) ) ;
#6363 = CIRCLE ( 'NONE', #992, 10.00000000000000178 ) ;
#6364 = STYLED_ITEM ( 'NONE', ( #6521 ), #11228 ) ;
#6365 = CARTESIAN_POINT ( 'NONE',  ( 0.000000000000000000, 65.00000000000000000, -75.00000000000002842 ) ) ;
#6366 = CARTESIAN_POINT ( 'NONE',  ( -34.80906958247980754, 75.85155757747834571, 7.997200496052795593 ) ) ;
#6367 = ORIENTED_EDGE ( 'NONE', *, *, #7016, .T. ) ;
#6368 = DIRECTION ( 'NONE',  ( 1.000000000000000000, 0.000000000000000000, 0.000000000000000000 ) ) ;
#6369 = DIRECTION ( 'NONE',  ( -0.000000000000000000, -1.000000000000000000, -0.000000000000000000 ) ) ;
#6370 = DIRECTION ( 'NONE',  ( 0.000000000000000000, 0.000000000000000000, -1.000000000000000000 ) ) ;
#6371 = CARTESIAN_POINT ( 'NONE',  ( 3.250000000000000444, 110.9374999972688016, 1.346194077712559167 ) ) ;
#6372 = ORIENTED_EDGE ( 'NONE', *, *, #5096, .T. ) ;
#6373 = CARTESIAN_POINT ( 'NONE',  ( 0.000000000000000000, 340.0000000000000000, 110.0000000000000284 ) ) ;
#6374 = DIRECTION ( 'NONE',  ( -0.000000000000000000, -1.000000000000000000, -0.000000000000000000 ) ) ;
#6375 = AXIS2_PLACEMENT_3D ( 'NONE', #2794, #11156, #11221 ) ;
#6376 =( REPRESENTATION_RELATIONSHIP ('NONE','NONE', #3713, #778 ) REPRESENTATION_RELATIONSHIP_WITH_TRANSFORMATION ( #9017 )SHAPE_REPRESENTATION_RELATIONSHIP( ) );
#6377 = CIRCLE ( 'NONE', #8554, 12.99999999999999822 ) ;
#6378 = VERTEX_POINT ( 'NONE', #5515 ) ;
#6379 = DIRECTION ( 'NONE',  ( 0.000000000000000000, 1.000000000000000000, 0.000000000000000000 ) ) ;
#6380 = LINE ( 'NONE', #11876, #11261 ) ;
#6381 = ORIENTED_EDGE ( 'NONE', *, *, #8252, .F. ) ;
#6382 = CARTESIAN_POINT ( 'NONE',  ( 0.000000000000000000, 75.00000000000001421, 0.000000000000000000 ) ) ;
#6383 = DIRECTION ( 'NONE',  ( -0.000000000000000000, -1.000000000000000000, -0.000000000000000000 ) ) ;
#6384 = VERTEX_POINT ( 'NONE', #1946 ) ;
#6385 = LINE ( 'NONE', #4799, #4422 ) ;
#6386 = VECTOR ( 'NONE', #1606, 1000.000000000000114 ) ;
#6387 = CARTESIAN_POINT ( 'NONE',  ( 9.184850993605150311E-15, 10.00000000000017586, -75.00000000000001421 ) ) ;
#6388 = ADVANCED_FACE ( 'NONE', ( #9476 ), #7557, .T. ) ;
#6389 = CARTESIAN_POINT ( 'NONE',  ( -1.121994411437820194, 112.2499999986344079, -2.708734124999999437 ) ) ;
#6390 = ORIENTED_EDGE ( 'NONE', *, *, #7267, .F. ) ;
#6391 = VECTOR ( 'NONE', #12191, 1000.000000000000114 ) ;
#6392 = FACE_OUTER_BOUND ( 'NONE', #6668, .T. ) ;
#6393 = LINE ( 'NONE', #3648, #3156 ) ;
#6394 = VECTOR ( 'NONE', #4884, 1000.000000000000000 ) ;
#6395 = EDGE_CURVE ( 'NONE', #3340, #2354, #3511, .T. ) ;
#6396 = DIRECTION ( 'NONE',  ( -0.000000000000000000, -0.000000000000000000, 1.000000000000000000 ) ) ;
#6397 = DIRECTION ( 'NONE',  ( 0.000000000000000000, -1.000000000000000000, -0.000000000000000000 ) ) ;
#6398 = EDGE_CURVE ( 'NONE', #4078, #3197, #8643, .T. ) ;
#6399 = CARTESIAN_POINT ( 'NONE',  ( -1.440781129305471087, 42.99759593155604875, 80.00000000000000000 ) ) ;
#6400 = VECTOR ( 'NONE', #9156, 1000.000000000000000 ) ;
#6401 = DIRECTION ( 'NONE',  ( -1.000000000000000000, 0.000000000000000000, 0.000000000000000000 ) ) ;
#6402 = CARTESIAN_POINT ( 'NONE',  ( -25.00000000000000000, 345.0000000000000568, -59.99999999999999289 ) ) ;
#6403 = CARTESIAN_POINT ( 'NONE',  ( 69.52686081652187511, 19.34506120843814614, -28.12500000000000000 ) ) ;
#6404 = ORIENTED_EDGE ( 'NONE', *, *, #9179, .T. ) ;
#6405 = CARTESIAN_POINT ( 'NONE',  ( -3.250000000000000444, 113.5000000000000000, 3.980102097228898231E-16 ) ) ;
#6406 = DIRECTION ( 'NONE',  ( 0.000000000000000000, -0.4999999999999976685, -0.8660254037844399289 ) ) ;
#6407 = VECTOR ( 'NONE', #2914, 1000.000000000000114 ) ;
#6408 = ADVANCED_FACE ( 'NONE', ( #5996 ), #254, .T. ) ;
#6409 = AXIS2_PLACEMENT_3D ( 'NONE', #7702, #86, #3712 ) ;
#6410 = CARTESIAN_POINT ( 'NONE',  ( 3.250000000000000444, 112.9374999972688016, 1.346194077712559167 ) ) ;
#6411 = ORIENTED_EDGE ( 'NONE', *, *, #770, .T. ) ;
#6412 = EDGE_CURVE ( 'NONE', #10667, #298, #11730, .T. ) ;
#6413 = ADVANCED_FACE ( 'NONE', ( #11675 ), #8788, .T. ) ;
#6414 = CARTESIAN_POINT ( 'NONE',  ( -9.726035167149728267, 35.21650635094616888, 79.50000000000000000 ) ) ;
#6415 = CARTESIAN_POINT ( 'NONE',  ( -24.76446302067273564, 285.0000000000000568, -102.0378428393002679 ) ) ;
#6416 = CARTESIAN_POINT ( 'NONE',  ( 74.30294665491157957, 18.67686843580081302, -24.82467190422460845 ) ) ;
#6417 = VERTEX_POINT ( 'NONE', #2944 ) ;
#6418 = DIRECTION ( 'NONE',  ( 0.4999999999999878431, -0.8660254037844455910, 0.000000000000000000 ) ) ;
#6419 = LINE ( 'NONE', #6539, #8535 ) ;
#6420 = ORIENTED_EDGE ( 'NONE', *, *, #7403, .T. ) ;
#6421 = DIRECTION ( 'NONE',  ( 1.000000000000000000, -0.000000000000000000, -0.000000000000000000 ) ) ;
#6422 = EDGE_CURVE ( 'NONE', #2329, #2084, #3065, .T. ) ;
#6423 = ORIENTED_EDGE ( 'NONE', *, *, #4461, .T. ) ;
#6424 = AXIS2_PLACEMENT_3D ( 'NONE', #2837, #10438, #6199 ) ;
#6425 = DIRECTION ( 'NONE',  ( 0.000000000000000000, 1.000000000000000000, 0.000000000000000000 ) ) ;
#6427 = ORIENTED_EDGE ( 'NONE', *, *, #10951, .T. ) ;
#6426 = CARTESIAN_POINT ( 'NONE',  ( 25.00000000000000000, 445.0000000000000568, -29.99999999999998934 ) ) ;
#6428 = VERTEX_POINT ( 'NONE', #8666 ) ;
#6429 = DIRECTION ( 'NONE',  ( 0.2500000000000003886, 6.938893903907242183E-16, 0.9682458365518542553 ) ) ;
#6430 = CARTESIAN_POINT ( 'NONE',  ( -20.00000000000000355, 7.965803112215716020, 57.08203932499370836 ) ) ;
#6431 = VERTEX_POINT ( 'NONE', #8844 ) ;
#6432 = DIRECTION ( 'NONE',  ( 0.7071067811865513475, 0.7071067811865437980, -0.000000000000000000 ) ) ;
#6433 = CARTESIAN_POINT ( 'NONE',  ( -7.474274778359196070, 18.61666975080236597, 79.50000000000000000 ) ) ;
#6434 = CARTESIAN_POINT ( 'NONE',  ( 72.61843774138907293, 50.00000000000000000, 18.75000000000000000 ) ) ;
#6435 = ORIENTED_EDGE ( 'NONE', *, *, #8750, .T. ) ;
#6436 = CARTESIAN_POINT ( 'NONE',  ( -1.121994411437820194, 112.2499999986344079, -2.708734124999999437 ) ) ;
#6437 = VECTOR ( 'NONE', #8773, 1000.000000000000000 ) ;
#6438 = DIRECTION ( 'NONE',  ( -0.000000000000000000, -0.000000000000000000, 1.000000000000000000 ) ) ;
#6439 = EDGE_CURVE ( 'NONE', #9777, #5376, #6987, .T. ) ;
#6440 = ORIENTED_EDGE ( 'NONE', *, *, #3154, .F. ) ;
#6441 = CARTESIAN_POINT ( 'NONE',  ( -1.357447795992929640, 17.00000000000009592, 80.00000048127353125 ) ) ;
#6442 = CARTESIAN_POINT ( 'NONE',  ( 2.500000000000000000, 0.000000000000000000, 0.000000000000000000 ) ) ;
#6443 = ORIENTED_EDGE ( 'NONE', *, *, #11700, .T. ) ;
#6444 = CARTESIAN_POINT ( 'NONE',  ( -3.250000000000001776, 112.5625000000000000, -1.346194077712558279 ) ) ;
#6445 = CARTESIAN_POINT ( 'NONE',  ( -20.00000000000000355, 7.965803112215716020, 57.08203932499370836 ) ) ;
#6446 = ORIENTED_EDGE ( 'NONE', *, *, #12178, .T. ) ;
#6447 = DIRECTION ( 'NONE',  ( 1.000000000000000000, -0.000000000000000000, 6.938893903907228378E-17 ) ) ;
#6448 = CARTESIAN_POINT ( 'NONE',  ( -9.726035167149728267, 35.21650635094616888, 79.50000000000000000 ) ) ;
#6449 = CARTESIAN_POINT ( 'NONE',  ( -2.708734124999999882, 111.9999999986343937, 1.121994411437818862 ) ) ;
#6450 = VERTEX_POINT ( 'NONE', #4064 ) ;
#6451 = EDGE_LOOP ( 'NONE', ( #11605, #2728 ) ) ;
#6452 = FILL_AREA_STYLE ('',( #8311 ) ) ;
#6453 = VECTOR ( 'NONE', #2026, 1000.000000000000000 ) ;
#6454 = AXIS2_PLACEMENT_3D ( 'NONE', #4616, #3503, #7308 ) ;
#6455 = EDGE_CURVE ( 'NONE', #4062, #7098, #188, .T. ) ;
#6456 = CARTESIAN_POINT ( 'NONE',  ( 0.000000000000000000, 170.0000000000000000, 0.000000000000000000 ) ) ;
#6457 = ADVANCED_FACE ( 'NONE', ( #1074 ), #128, .F. ) ;
#6458 = FACE_OUTER_BOUND ( 'NONE', #10995, .T. ) ;
#6459 = CARTESIAN_POINT ( 'NONE',  ( -31.52024609858349180, 77.00000000000001421, 7.288261850756687643 ) ) ;
#6460 = DIRECTION ( 'NONE',  ( 0.5000000000000066613, 0.8660254037844347108, 0.000000000000000000 ) ) ;
#6461 = LINE ( 'NONE', #12014, #8654 ) ;
#6462 = CARTESIAN_POINT ( 'NONE',  ( -2.076303083421399354, 44.98277681526300853, 74.97303962124122734 ) ) ;
#6463 = CARTESIAN_POINT ( 'NONE',  ( 0.000000000000000000, 65.00000000000000000, 0.000000000000000000 ) ) ;
#6464 = AXIS2_PLACEMENT_3D ( 'NONE', #373, #4124, #6989 ) ;
#6465 = ORIENTED_EDGE ( 'NONE', *, *, #7466, .F. ) ;
#6466 = CARTESIAN_POINT ( 'NONE',  ( -12.57411137850303540, 36.28349364905398033, 79.50000000000000000 ) ) ;
#6467 = DIRECTION ( 'NONE',  ( -0.000000000000000000, -1.000000000000000000, -0.000000000000000000 ) ) ;
#6468 = EDGE_CURVE ( 'NONE', #8398, #8933, #2284, .T. ) ;
#6469 = VECTOR ( 'NONE', #2991, 1000.000000000000000 ) ;
#6470 = LINE ( 'NONE', #12090, #5218 ) ;
#6471 = AXIS2_PLACEMENT_3D ( 'NONE', #389, #5083, #5323 ) ;
#6472 = VERTEX_POINT ( 'NONE', #2187 ) ;
#6473 = CARTESIAN_POINT ( 'NONE',  ( 0.000000000000000000, 65.00000000000000000, -73.00000000000002842 ) ) ;
#6474 = ADVANCED_FACE ( 'NONE', ( #10666 ), #2069, .T. ) ;
#6475 = DIRECTION ( 'NONE',  ( 0.000000000000000000, 0.000000000000000000, -1.000000000000000000 ) ) ;
#6476 = DIRECTION ( 'NONE',  ( 0.000000000000000000, 0.000000000000000000, -1.000000000000000000 ) ) ;
#6477 = ORIENTED_EDGE ( 'NONE', *, *, #10812, .T. ) ;
#6478 = CARTESIAN_POINT ( 'NONE',  ( 27.02024436599224444, 275.0000000000000000, -111.3324139431193203 ) ) ;
#6479 = DIRECTION ( 'NONE',  ( -0.000000000000000000, -1.000000000000000000, -0.000000000000000000 ) ) ;
#6480 = CIRCLE ( 'NONE', #5097, 9.999999999999998224 ) ;
#6481 = ORIENTED_EDGE ( 'NONE', *, *, #8736, .T. ) ;
#6482 = CARTESIAN_POINT ( 'NONE',  ( -6.000000000000000000, 50.00000000000000000, 69.74238309665079782 ) ) ;
#6483 = AXIS2_PLACEMENT_3D ( 'NONE', #7055, #11926, #505 ) ;
#6484 = EDGE_CURVE ( 'NONE', #2099, #2436, #10842, .T. ) ;
#6485 = EDGE_CURVE ( 'NONE', #6472, #1199, #11857, .T. ) ;
#6486 = EDGE_LOOP ( 'NONE', ( #6206, #4628, #8800, #8607, #2421 ) ) ;
#6487 = EDGE_LOOP ( 'NONE', ( #5447, #2294, #151, #12318 ) ) ;
#6488 = DIRECTION ( 'NONE',  ( 1.224646799147349509E-16, 0.000000000000000000, -1.000000000000000000 ) ) ;
#6490 = ORIENTED_EDGE ( 'NONE', *, *, #1441, .T. ) ;
#6489 = DIRECTION ( 'NONE',  ( 0.000000000000000000, 0.000000000000000000, 1.000000000000000000 ) ) ;
#6491 = ORIENTED_EDGE ( 'NONE', *, *, #4115, .T. ) ;
#6492 = CIRCLE ( 'NONE', #1116, 5.000000000000004441 ) ;
#6493 = DIRECTION ( 'NONE',  ( 0.000000000000000000, 0.4999999999999965028, -0.8660254037844407060 ) ) ;
#6494 = CARTESIAN_POINT ( 'NONE',  ( -28.47250777504872943, 87.47929846073044757, -9.490423323819145551 ) ) ;
#6495 = ORIENTED_EDGE ( 'NONE', *, *, #3164, .T. ) ;
#6496 = CARTESIAN_POINT ( 'NONE',  ( -27.67899820261485999, 88.38261385519929547, -11.05501148229834030 ) ) ;
#6497 = AXIS2_PLACEMENT_3D ( 'NONE', #4291, #6109, #12094 ) ;
#6498 = CARTESIAN_POINT ( 'NONE',  ( -30.00100000000000122, 85.26794919243110371, 9.660254037844429931 ) ) ;
#6499 = LINE ( 'NONE', #11359, #4208 ) ;
#6500 = PRODUCT_RELATED_PRODUCT_CATEGORY ( 'part', '', ( #10662 ) ) ;
#6501 = EDGE_LOOP ( 'NONE', ( #5142, #8644, #8020, #3019 ) ) ;
#6502 = CARTESIAN_POINT ( 'NONE',  ( 2.708734124999999882, 113.5624999986344079, 0.000000000000000000 ) ) ;
#6503 = DIRECTION ( 'NONE',  ( -0.000000000000000000, 1.000000000000000000, -0.000000000000000000 ) ) ;
#6504 = CIRCLE ( 'NONE', #4505, 40.00000000000000000 ) ;
#6505 = ORIENTED_EDGE ( 'NONE', *, *, #8093, .F. ) ;
#6506 = CARTESIAN_POINT ( 'NONE',  ( -20.00000000000000000, 54.99999999999999289, 67.08203932499370126 ) ) ;
#6507 = CARTESIAN_POINT ( 'NONE',  ( 69.52686081652188932, 40.65493879156205281, 28.12500000000001066 ) ) ;
#6508 = VERTEX_POINT ( 'NONE', #8095 ) ;
#6509 = CARTESIAN_POINT ( 'NONE',  ( -2.298097038856279806, 112.6250000000000000, -2.298097038856279362 ) ) ;
#6510 = CARTESIAN_POINT ( 'NONE',  ( 76.84714931290172046, 44.87559967700520502, 21.12007276954038915 ) ) ;
#6511 = EDGE_LOOP ( 'NONE', ( #2573, #5903, #3946, #9083, #10917 ) ) ;
#6512 = ADVANCED_FACE ( 'NONE', ( #7971 ), #4471, .F. ) ;
#6513 = CARTESIAN_POINT ( 'NONE',  ( -25.00000000000000000, 445.0000000000000568, -31.99999999999999289 ) ) ;
#6514 = CARTESIAN_POINT ( 'NONE',  ( 0.000000000000000000, 77.00000000000000000, -25.50000000000000000 ) ) ;
#6515 = CARTESIAN_POINT ( 'NONE',  ( 1.121994411437819084, 111.3749999986344221, -2.708734124999999437 ) ) ;
#6516 = AXIS2_PLACEMENT_3D ( 'NONE', #1023, #4822, #7562 ) ;
#6517 = FACE_OUTER_BOUND ( 'NONE', #1628, .T. ) ;
#6518 = ADVANCED_FACE ( 'NONE', ( #7171 ), #3090, .F. ) ;
#6519 = ORIENTED_EDGE ( 'NONE', *, *, #6608, .T. ) ;
#6520 = ORIENTED_EDGE ( 'NONE', *, *, #6540, .T. ) ;
#6521 = PRESENTATION_STYLE_ASSIGNMENT (( #1591 ) ) ;
#6522 = CARTESIAN_POINT ( 'NONE',  ( -89.80805993797480369, 275.0000000000000000, 71.82974571984181011 ) ) ;
#6523 = DIRECTION ( 'NONE',  ( -0.2358520287683116834, 0.000000000000000000, 0.9717889794219068955 ) ) ;
#6524 = ORIENTED_EDGE ( 'NONE', *, *, #11109, .T. ) ;
#6525 = DIRECTION ( 'NONE',  ( 0.000000000000000000, 0.000000000000000000, 1.000000000000000000 ) ) ;
#6526 = CARTESIAN_POINT ( 'NONE',  ( 8.817456953860944867E-15, 52.00000000000000711, 72.00000000000002842 ) ) ;
#6527 = LINE ( 'NONE', #11622, #500 ) ;
#6528 = CARTESIAN_POINT ( 'NONE',  ( -8.022189948025989281, 43.39365864146846263, 74.57502254044544543 ) ) ;
#6529 = DIRECTION ( 'NONE',  ( -0.000000000000000000, 1.000000000000000000, -0.000000000000000000 ) ) ;
#6530 = CYLINDRICAL_SURFACE ( 'NONE', #5981, 110.0000000000000284 ) ;
#6531 = CARTESIAN_POINT ( 'NONE',  ( 7.007733291640687590, 17.40453028225516974, 74.67565132020823171 ) ) ;
#6532 = VERTEX_POINT ( 'NONE', #4178 ) ;
#6533 = AXIS2_PLACEMENT_3D ( 'NONE', #370, #252, #3242 ) ;
#6534 = LINE ( 'NONE', #6414, #669 ) ;
#6535 = DIRECTION ( 'NONE',  ( -0.000000000000000000, -1.000000000000000000, -0.000000000000000000 ) ) ;
#6536 = DIRECTION ( 'NONE',  ( 0.000000000000000000, 0.000000000000000000, -1.000000000000000000 ) ) ;
#6537 = ORIENTED_EDGE ( 'NONE', *, *, #154, .T. ) ;
#6538 = CARTESIAN_POINT ( 'NONE',  ( 27.69110892066590779, 86.46107124639162578, 11.72680205493499628 ) ) ;
#6539 = CARTESIAN_POINT ( 'NONE',  ( -11.19078112930532498, 30.25000000000005684, 79.50000000000000000 ) ) ;
#6540 = EDGE_CURVE ( 'NONE', #7450, #1004, #8217, .T. ) ;
#6541 = ORIENTED_EDGE ( 'NONE', *, *, #5783, .F. ) ;
#6542 = DIRECTION ( 'NONE',  ( -1.000000000000000000, 0.000000000000000000, 0.000000000000000000 ) ) ;
#6543 = AXIS2_PLACEMENT_3D ( 'NONE', #11005, #2468, #10060 ) ;
#6544 = ORIENTED_EDGE ( 'NONE', *, *, #39, .T. ) ;
#6545 = DIRECTION ( 'NONE',  ( 0.000000000000000000, 1.000000000000000000, 0.000000000000000000 ) ) ;
#6546 = DIRECTION ( 'NONE',  ( 0.000000000000000000, 1.000000000000000000, 0.000000000000000000 ) ) ;
#6547 = ORIENTED_EDGE ( 'NONE', *, *, #4136, .F. ) ;
#6548 = PLANE ( 'NONE',  #3305 ) ;
#6549 = ORIENTED_EDGE ( 'NONE', *, *, #9770, .T. ) ;
#6550 = EDGE_CURVE ( 'NONE', #9788, #421, #1239, .T. ) ;
#6551 = EDGE_CURVE ( 'NONE', #2768, #1231, #1846, .T. ) ;
#6552 = CARTESIAN_POINT ( 'NONE',  ( 97.61745645431939522, 285.0000000000000568, 78.07581056504676553 ) ) ;
#6553 = CARTESIAN_POINT ( 'NONE',  ( -30.00100000000000122, 77.00000000000000000, -8.660254037844445918 ) ) ;
#6554 = CARTESIAN_POINT ( 'NONE',  ( -25.00000000000000000, 445.0000000000000568, -24.99999999999998934 ) ) ;
#6555 = VERTEX_POINT ( 'NONE', #4239 ) ;
#6556 = CARTESIAN_POINT ( 'NONE',  ( -1.915364268218908927, 111.9374999986344079, 1.915364268218909150 ) ) ;
#6557 = VECTOR ( 'NONE', #2031, 1000.000000000000000 ) ;
#6558 = EDGE_CURVE ( 'NONE', #5372, #10740, #9906, .T. ) ;
#6559 = EDGE_LOOP ( 'NONE', ( #1144, #6170, #4035, #3338 ) ) ;
#6560 = FACE_OUTER_BOUND ( 'NONE', #5800, .T. ) ;
#6561 = CARTESIAN_POINT ( 'NONE',  ( -14.50972348255446320, 23.02286878654513202, 73.58429599720173542 ) ) ;
#6562 = ORIENTED_EDGE ( 'NONE', *, *, #11915, .T. ) ;
#6563 = LINE ( 'NONE', #7559, #9227 ) ;
#6564 = DIRECTION ( 'NONE',  ( -0.000000000000000000, -0.000000000000000000, 1.000000000000000000 ) ) ;
#6565 = ORIENTED_EDGE ( 'NONE', *, *, #9080, .F. ) ;
#6566 = DIRECTION ( 'NONE',  ( 0.000000000000000000, 0.000000000000000000, -1.000000000000000000 ) ) ;
#6567 = FACE_OUTER_BOUND ( 'NONE', #3381, .T. ) ;
#6568 = AXIS2_PLACEMENT_3D ( 'NONE', #2922, #3041, #10581 ) ;
#6569 = CARTESIAN_POINT ( 'NONE',  ( -1.915364268218909594, 111.1874999986344079, -1.915364268218908927 ) ) ;
#6570 = DIRECTION ( 'NONE',  ( -3.469446951953613203E-16, 0.000000000000000000, -1.000000000000000000 ) ) ;
#6571 = EDGE_LOOP ( 'NONE', ( #2515, #6646, #10925, #1490 ) ) ;
#6572 =( NAMED_UNIT ( * ) PLANE_ANGLE_UNIT ( ) SI_UNIT ( $, .RADIAN. ) );
#6573 = EDGE_CURVE ( 'NONE', #8283, #8585, #2845, .T. ) ;
#6574 = ADVANCED_FACE ( 'NONE', ( #3439 ), #1502, .T. ) ;
#6575 = AXIS2_PLACEMENT_3D ( 'NONE', #2509, #5256, #9159 ) ;
#6576 = DIRECTION ( 'NONE',  ( 0.000000000000000000, 0.000000000000000000, -1.000000000000000000 ) ) ;
#6577 = DIRECTION ( 'NONE',  ( 0.000000000000000000, 0.000000000000000000, -1.000000000000000000 ) ) ;
#6578 = ORIENTED_EDGE ( 'NONE', *, *, #3046, .T. ) ;
#6579 = DIRECTION ( 'NONE',  ( 0.8660254037844424824, 0.4999999999999933387, 0.000000000000000000 ) ) ;
#6580 = DIRECTION ( 'NONE',  ( 0.000000000000000000, 0.000000000000000000, 1.000000000000000000 ) ) ;
#6581 = CARTESIAN_POINT ( 'NONE',  ( -14.01037901404159669, 37.85720668004749712, 73.68231848073395440 ) ) ;
#6582 = DIRECTION ( 'NONE',  ( 0.000000000000000000, 0.000000000000000000, 1.000000000000000000 ) ) ;
#6583 = ORIENTED_EDGE ( 'NONE', *, *, #5646, .T. ) ;
#6584 = AXIS2_PLACEMENT_3D ( 'NONE', #4633, #963, #9358 ) ;
#6585 = AXIS2_PLACEMENT_3D ( 'NONE', #10378, #1666, #5658 ) ;
#6586 = FACE_OUTER_BOUND ( 'NONE', #6976, .T. ) ;
#6587 = CARTESIAN_POINT ( 'NONE',  ( 70.87894850892848808, 41.68318366108226058, -24.74065748999147019 ) ) ;
#6588 = CARTESIAN_POINT ( 'NONE',  ( 75.00000000000001421, 15.00000000000008882, 20.00000000000000000 ) ) ;
#6589 = ORIENTED_EDGE ( 'NONE', *, *, #7837, .F. ) ;
#6590 = VECTOR ( 'NONE', #444, 1000.000000000000114 ) ;
#6591 = TOROIDAL_SURFACE ( 'NONE', #5604, 25.00000000000000000, 10.00000000000000000 ) ;
#6592 = DIRECTION ( 'NONE',  ( -0.000000000000000000, -1.000000000000000000, -0.000000000000000000 ) ) ;
#6593 = LINE ( 'NONE', #3347, #2692 ) ;
#6594 = CARTESIAN_POINT ( 'NONE',  ( 24.76446302067270722, 275.0000000000000000, -102.0378428393002679 ) ) ;
#6595 = ORIENTED_EDGE ( 'NONE', *, *, #6127, .T. ) ;
#6596 = DIRECTION ( 'NONE',  ( -1.000000000000000000, -0.000000000000000000, -0.000000000000000000 ) ) ;
#6597 = DIRECTION ( 'NONE',  ( 0.000000000000000000, 0.000000000000000000, -1.000000000000000000 ) ) ;
#6598 = VECTOR ( 'NONE', #6058, 1000.000000000000000 ) ;
#6599 = ORIENTED_EDGE ( 'NONE', *, *, #1623, .F. ) ;
#6600 = CARTESIAN_POINT ( 'NONE',  ( -1.190781129305471087, 30.00000000000008882, 65.00000000000000000 ) ) ;
#6601 = VECTOR ( 'NONE', #2937, 1000.000000000000000 ) ;
#6602 = ADVANCED_FACE ( 'NONE', ( #4358, #7235 ), #11800, .F. ) ;
#6603 = ORIENTED_EDGE ( 'NONE', *, *, #3487, .T. ) ;
#6604 = ADVANCED_FACE ( 'NONE', ( #5185 ), #11101, .T. ) ;
#6605 = DIRECTION ( 'NONE',  ( 1.224646799147352468E-16, 0.000000000000000000, -1.000000000000000000 ) ) ;
#6606 = DIRECTION ( 'NONE',  ( 0.000000000000000000, -0.8660254037844401509, 0.4999999999999974465 ) ) ;
#6607 = ORIENTED_EDGE ( 'NONE', *, *, #2337, .F. ) ;
#6608 = EDGE_CURVE ( 'NONE', #7410, #2768, #8803, .T. ) ;
#6609 = CARTESIAN_POINT ( 'NONE',  ( 34.17938886450476588, 77.00000000000000000, -8.633741422215349459 ) ) ;
#6610 = ORIENTED_EDGE ( 'NONE', *, *, #4703, .T. ) ;
#6611 = DIRECTION ( 'NONE',  ( 0.000000000000000000, 0.000000000000000000, 1.000000000000000000 ) ) ;
#6612 = LINE ( 'NONE', #9466, #1703 ) ;
#6613 = LINE ( 'NONE', #9590, #6601 ) ;
#6614 = DIRECTION ( 'NONE',  ( 6.938893903907221475E-16, 0.000000000000000000, -1.000000000000000000 ) ) ;
#6615 = ORIENTED_EDGE ( 'NONE', *, *, #608, .T. ) ;
#6616 = CARTESIAN_POINT ( 'NONE',  ( -1.915364268218909594, 114.1874999986344079, -1.915364268218908927 ) ) ;
#6617 = CARTESIAN_POINT ( 'NONE',  ( 3.250000000000000444, 112.9374999972688016, 1.346194077712559389 ) ) ;
#6618 = AXIS2_PLACEMENT_3D ( 'NONE', #4582, #9183, #10119 ) ;
#6619 = VERTEX_POINT ( 'NONE', #437 ) ;
#6620 = EDGE_CURVE ( 'NONE', #1577, #10879, #1254, .T. ) ;
#6621 = DIRECTION ( 'NONE',  ( 0.000000000000000000, 0.000000000000000000, 1.000000000000000000 ) ) ;
#6622 = CARTESIAN_POINT ( 'NONE',  ( 70.48329812536721306, 46.79482878816214253, 25.63505613512332459 ) ) ;
#6623 = ORIENTED_EDGE ( 'NONE', *, *, #365, .T. ) ;
#6624 = CARTESIAN_POINT ( 'NONE',  ( 10.19254911989241386, 23.71650635094626836, 79.50000000000000000 ) ) ;
#6625 = CARTESIAN_POINT ( 'NONE',  ( 77.29209776116496755, 45.00000000000009237, 20.32449628861576940 ) ) ;
#6626 = ORIENTED_EDGE ( 'NONE', *, *, #5905, .F. ) ;
#6627 = EDGE_CURVE ( 'NONE', #6899, #2508, #2841, .T. ) ;
#6628 = DIRECTION ( 'NONE',  ( 0.000000000000000000, 1.000000000000000000, 0.000000000000000000 ) ) ;
#6629 = DIRECTION ( 'NONE',  ( 0.000000000000000000, 1.000000000000000000, 0.000000000000000000 ) ) ;
#6630 = AXIS2_PLACEMENT_3D ( 'NONE', #11845, #8142, #4226 ) ;
#6631 = DIRECTION ( 'NONE',  ( -0.000000000000000000, 1.000000000000000000, -0.000000000000000000 ) ) ;
#6632 = DIRECTION ( 'NONE',  ( 1.000000000000000000, -1.040834085586083310E-14, 0.000000000000000000 ) ) ;
#6633 = ORIENTED_EDGE ( 'NONE', *, *, #3640, .T. ) ;
#6634 = SURFACE_STYLE_FILL_AREA ( #2832 ) ;
#6635 = EDGE_CURVE ( 'NONE', #1312, #4833, #6117, .T. ) ;
#6636 = ADVANCED_FACE ( 'NONE', ( #9459 ), #3048, .F. ) ;
#6637 = ORIENTED_EDGE ( 'NONE', *, *, #4016, .T. ) ;
#6638 = CIRCLE ( 'NONE', #1471, 12.99999999999999822 ) ;
#6639 = CARTESIAN_POINT ( 'NONE',  ( -12.57202939415816267, 36.28229161483201892, 80.00000000000000000 ) ) ;
#6640 = VERTEX_POINT ( 'NONE', #11410 ) ;
#6641 = DIRECTION ( 'NONE',  ( 0.000000000000000000, 1.000000000000000000, 0.000000000000000000 ) ) ;
#6642 = DIRECTION ( 'NONE',  ( 1.224646799147352714E-16, 0.000000000000000000, -1.000000000000000000 ) ) ;
#6643 =( BOUNDED_CURVE ( )  B_SPLINE_CURVE ( 2, ( #8671, #133, #1263, #4947, #3948, #7743, #8793, #4007, #11557 ),
 .UNSPECIFIED., .F., .F. ) 
 B_SPLINE_CURVE_WITH_KNOTS ( ( 3, 2, 2, 2, 3 ),
 ( 0.06250000000000005551, 0.09375000000000008327, 0.1250000000000001110, 0.1562500000000001388, 0.1875000000000001665 ),
 .UNSPECIFIED. ) 
 CURVE ( )  GEOMETRIC_REPRESENTATION_ITEM ( )  RATIONAL_B_SPLINE_CURVE ( ( 0.9999999999999998890, 0.9238795325112868495, 1.000000000000000000, 0.9238795325112867385, 1.000000000000000000, 0.9238795325112867385, 1.000000000000000000, 0.9238795325112862944, 1.000000000000000444 ) ) 
 REPRESENTATION_ITEM ( '' )  );
#6644 = DIRECTION ( 'NONE',  ( -0.000000000000000000, 1.000000000000000000, -0.000000000000000000 ) ) ;
#6645 = DIRECTION ( 'NONE',  ( 0.4999999999999878431, -0.8660254037844455910, 0.000000000000000000 ) ) ;
#6646 = ORIENTED_EDGE ( 'NONE', *, *, #8965, .T. ) ;
#6647 = UNCERTAINTY_MEASURE_WITH_UNIT (LENGTH_MEASURE( 1.000000000000000082E-05 ), #5743, 'distance_accuracy_value', 'NONE');
#6648 = CARTESIAN_POINT ( 'NONE',  ( 69.65391855624119444, 42.66023882883560248, -27.80917345409739383 ) ) ;
#6649 = CARTESIAN_POINT ( 'NONE',  ( -25.00000000000000000, 450.0000000000000568, -59.99999999999999289 ) ) ;
#6650 = EDGE_LOOP ( 'NONE', ( #12069, #6547, #3960, #4039 ) ) ;
#6651 = CARTESIAN_POINT ( 'NONE',  ( 3.980102097228898231E-16, 110.0000000000000000, -3.250000000000000444 ) ) ;
#6652 = AXIS2_PLACEMENT_3D ( 'NONE', #5326, #4510, #10926 ) ;
#6653 = VECTOR ( 'NONE', #1677, 1000.000000000000000 ) ;
#6654 = CARTESIAN_POINT ( 'NONE',  ( -34.84121487603211875, 75.26794919243111792, 7.660254037844449471 ) ) ;
#6655 = FACE_OUTER_BOUND ( 'NONE', #5557, .T. ) ;
#6656 = ORIENTED_EDGE ( 'NONE', *, *, #8954, .T. ) ;
#6657 = CARTESIAN_POINT ( 'NONE',  ( 0.000000000000000000, 92.00000000000000000, 0.000000000000000000 ) ) ;
#6658 = EDGE_CURVE ( 'NONE', #6384, #10790, #10334, .T. ) ;
#6659 = CARTESIAN_POINT ( 'NONE',  ( 2.708734125000000326, 110.3124999986344079, 0.000000000000000000 ) ) ;
#6660 = VERTEX_POINT ( 'NONE', #2616 ) ;
#6661 = CARTESIAN_POINT ( 'NONE',  ( 165.0000000000011369, 0.000000000000000000, 20.00000000000000000 ) ) ;
#6662 = EDGE_CURVE ( 'NONE', #5753, #5494, #1806, .T. ) ;
#6663 =( BOUNDED_CURVE ( )  B_SPLINE_CURVE ( 2, ( #6344, #8326, #859, #1547, #10260, #6410, #11276, #10197, #1733 ),
 .UNSPECIFIED., .F., .F. ) 
 B_SPLINE_CURVE_WITH_KNOTS ( ( 3, 2, 2, 2, 3 ),
 ( 0.4375000000000003886, 0.4687500000000003886, 0.5000000000000004441, 0.5312500000000004441, 0.5625000000000004441 ),
 .UNSPECIFIED. ) 
 CURVE ( )  GEOMETRIC_REPRESENTATION_ITEM ( )  RATIONAL_B_SPLINE_CURVE ( ( 0.9999999999999990008, 0.9238795325112877377, 1.000000000000000000, 0.9238795325112867385, 1.000000000000000000, 0.9238795325112867385, 1.000000000000000000, 0.9238795325112856283, 1.000000000000001110 ) ) 
 REPRESENTATION_ITEM ( '' )  );
#6664 = AXIS2_PLACEMENT_3D ( 'NONE', #11920, #5246, #371 ) ;
#6665 = VERTEX_POINT ( 'NONE', #8404 ) ;
#6666 = DIRECTION ( 'NONE',  ( 1.224646799147352961E-16, 0.000000000000000000, -1.000000000000000000 ) ) ;
#6667 = CARTESIAN_POINT ( 'NONE',  ( 121.4644660940682428, 46.46446609406732620, 25.00000000000000000 ) ) ;
#6668 = EDGE_LOOP ( 'NONE', ( #3629, #4876, #6177, #11936 ) ) ;
#6669 = DIRECTION ( 'NONE',  ( 0.000000000000000000, 1.000000000000000000, 0.000000000000000000 ) ) ;
#6670 = CARTESIAN_POINT ( 'NONE',  ( 0.000000000000000000, -5.000000000000000000, -65.00000000000001421 ) ) ;
#6671 = VERTEX_POINT ( 'NONE', #6426 ) ;
#6672 = TOROIDAL_SURFACE ( 'NONE', #4489, 90.00000000000002842, 8.000000000000000000 ) ;
#6673 = PLANE ( 'NONE',  #11459 ) ;
#6674 = LINE ( 'NONE', #7731, #5621 ) ;
#6675 = CARTESIAN_POINT ( 'NONE',  ( 0.000000000000000000, 265.0000000000000000, 0.000000000000000000 ) ) ;
#6676 = EDGE_CURVE ( 'NONE', #3231, #2119, #5444, .T. ) ;
#6677 = EDGE_LOOP ( 'NONE', ( #6440, #9582, #11470, #9849, #11661 ) ) ;
#6678 = CARTESIAN_POINT ( 'NONE',  ( 2.708734124999999437, 112.4999999986344079, -1.121994411437820638 ) ) ;
#6679 = CARTESIAN_POINT ( 'NONE',  ( -3.250000000000000444, 111.3124999972687874, 1.346194077712559389 ) ) ;
#6680 = PRESENTATION_LAYER_ASSIGNMENT (  '', '', ( #2896 ) ) ;
#6681 = PRODUCT_DEFINITION_SHAPE ( 'NONE', 'NONE',  #5048 ) ;
#6682 = ADVANCED_FACE ( 'NONE', ( #1627 ), #10212, .T. ) ;
#6683 = CIRCLE ( 'NONE', #3893, 70.00000000000000000 ) ;
#6684 = ORIENTED_EDGE ( 'NONE', *, *, #1029, .F. ) ;
#6685 = DIRECTION ( 'NONE',  ( -0.000000000000000000, -0.000000000000000000, 1.000000000000000000 ) ) ;
#6686 = PLANE ( 'NONE',  #2493 ) ;
#6687 = ORIENTED_EDGE ( 'NONE', *, *, #8578, .F. ) ;
#6688 = AXIS2_PLACEMENT_3D ( 'NONE', #8180, #12350, #9521 ) ;
#6689 = FACE_OUTER_BOUND ( 'NONE', #8966, .T. ) ;
#6690 = CARTESIAN_POINT ( 'NONE',  ( 70.01409082250445692, 15.02759043508419623, 26.88960057466318077 ) ) ;
#6691 = EDGE_LOOP ( 'NONE', ( #1761, #4157, #2453, #2487, #10628, #8114 ) ) ;
#6692 = LINE ( 'NONE', #1083, #6314 ) ;
#6693 = PLANE ( 'NONE',  #5398 ) ;
#6694 = AXIS2_PLACEMENT_3D ( 'NONE', #4183, #6243, #7174 ) ;
#6695 = DIRECTION ( 'NONE',  ( -1.000000000000000000, 0.000000000000000000, 0.000000000000000000 ) ) ;
#6696 = CARTESIAN_POINT ( 'NONE',  ( -1.346194077712559389, 113.3125000000000142, 3.250000000000000444 ) ) ;
#6697 = EDGE_CURVE ( 'NONE', #7931, #5487, #2675, .T. ) ;
#6698 = CARTESIAN_POINT ( 'NONE',  ( -4.975863863883684959E-16, 114.3124999986344079, -2.708734124999999882 ) ) ;
#6699 = EDGE_LOOP ( 'NONE', ( #9477, #11821, #2677, #1944, #8464, #4202, #7418 ) ) ;
#6700 = AXIS2_PLACEMENT_3D ( 'NONE', #10874, #3335, #11698 ) ;
#6701 = ORIENTED_EDGE ( 'NONE', *, *, #7862, .T. ) ;
#6702 = CARTESIAN_POINT ( 'NONE',  ( 41.03553390593253170, -41.03553390593296513, 20.00000000000000000 ) ) ;
#6703 = CARTESIAN_POINT ( 'NONE',  ( 0.000000000000000000, 122.0000000000000000, 0.000000000000000000 ) ) ;
#6704 = ORIENTED_EDGE ( 'NONE', *, *, #11318, .T. ) ;
#6705 = FACE_OUTER_BOUND ( 'NONE', #2089, .T. ) ;
#6706 = CARTESIAN_POINT ( 'NONE',  ( 45.35898384862240107, 86.99999999999997158, 8.660254037844424602 ) ) ;
#6707 = VECTOR ( 'NONE', #840, 1000.000000000000000 ) ;
#6708 = CARTESIAN_POINT ( 'NONE',  ( -12.36577804515927070, 36.64433756731555292, 80.00000048127353125 ) ) ;
#6709 = LINE ( 'NONE', #9560, #6021 ) ;
#6710 = EDGE_CURVE ( 'NONE', #9853, #3368, #11002, .T. ) ;
#6711 = AXIS2_PLACEMENT_3D ( 'NONE', #4366, #12174, #3446 ) ;
#6712 = EDGE_CURVE ( 'NONE', #8932, #5022, #940, .T. ) ;
#6713 = CARTESIAN_POINT ( 'NONE',  ( 70.79098555864042908, 40.00000000000007816, -25.00000000000000000 ) ) ;
#6714 = B_SPLINE_CURVE_WITH_KNOTS ( 'NONE', 3,
 ( #11476, #2928, #10525, #1184, #1991, #4986, #5799, #1057, #3928, #2989, #7723, #10589, #5859, #9642, #4926, #10075, #6106, #6224 ),
 .UNSPECIFIED., .F., .F.,
 ( 4, 2, 2, 2, 2, 2, 2, 2, 4 ),
 ( 0.000000000000000000, 0.001070893387785250587, 0.002141786775570501174, 0.003212680163355751545, 0.004283573551141002349, 0.005354466938926253153, 0.006425360326711503089, 0.007496253714496753894, 0.008567147102282004698 ),
 .UNSPECIFIED. ) ;
#6715 = FACE_OUTER_BOUND ( 'NONE', #10568, .T. ) ;
#6716 = LINE ( 'NONE', #11164, #12181 ) ;
#6717 = CARTESIAN_POINT ( 'NONE',  ( 9.184850993605150311E-15, 50.00000000000000000, 75.00000000000001421 ) ) ;
#6718 = DIRECTION ( 'NONE',  ( -0.5000000000000005551, -0.8660254037844382635, 0.000000000000000000 ) ) ;
#6719 = ORIENTED_EDGE ( 'NONE', *, *, #3352, .F. ) ;
#6720 = DIRECTION ( 'NONE',  ( 0.000000000000000000, 0.000000000000000000, 1.000000000000000000 ) ) ;
#6721 = CARTESIAN_POINT ( 'NONE',  ( 0.000000000000000000, 260.0000000000000000, 0.000000000000000000 ) ) ;
#6722 = EDGE_LOOP ( 'NONE', ( #7835, #494, #11465, #7561 ) ) ;
#6723 = CARTESIAN_POINT ( 'NONE',  ( 0.000000000000000000, 216.0365690573663926, 0.000000000000000000 ) ) ;
#6724 = EDGE_CURVE ( 'NONE', #9423, #10953, #5676, .T. ) ;
#6725 = EDGE_LOOP ( 'NONE', ( #2372, #5808, #4587, #9264, #394 ) ) ;
#6726 = EDGE_CURVE ( 'NONE', #6910, #5955, #10277, .T. ) ;
#6727 = DIRECTION ( 'NONE',  ( 0.000000000000000000, 1.000000000000000000, 0.000000000000000000 ) ) ;
#6728 = DIRECTION ( 'NONE',  ( 0.000000000000000000, 0.000000000000000000, -1.000000000000000000 ) ) ;
#6729 = ORIENTED_EDGE ( 'NONE', *, *, #10963, .F. ) ;
#6730 = DIRECTION ( 'NONE',  ( -1.000000000000000000, 0.000000000000000000, 0.000000000000000000 ) ) ;
#6731 = LINE ( 'NONE', #5924, #924 ) ;
#6732 = ORIENTED_EDGE ( 'NONE', *, *, #7726, .F. ) ;
#6733 = ADVANCED_FACE ( 'NONE', ( #2737 ), #11349, .F. ) ;
#6734 =( NAMED_UNIT ( * ) PLANE_ANGLE_UNIT ( ) SI_UNIT ( $, .RADIAN. ) );
#6735 = FACE_OUTER_BOUND ( 'NONE', #9169, .T. ) ;
#6736 = CARTESIAN_POINT ( 'NONE',  ( 25.00000000000000000, 450.0000000000000568, -59.99999999999999289 ) ) ;
#6737 = CARTESIAN_POINT ( 'NONE',  ( 30.00100000000000122, 77.00000000000000000, 4.660254037844413944 ) ) ;
#6738 = CIRCLE ( 'NONE', #4146, 5.000000000000004441 ) ;
#6739 = ORIENTED_EDGE ( 'NONE', *, *, #9902, .F. ) ;
#6740 = CARTESIAN_POINT ( 'NONE',  ( -2.708734125000000326, 110.8124999986344079, 3.317242575922457132E-16 ) ) ;
#6741 = CARTESIAN_POINT ( 'NONE',  ( 1.346194077712559833, 111.6874999972688016, -3.250000000000000000 ) ) ;
#6742 = ORIENTED_EDGE ( 'NONE', *, *, #8751, .T. ) ;
#6743 = DIRECTION ( 'NONE',  ( 6.938893903907229610E-17, 0.000000000000000000, -1.000000000000000000 ) ) ;
#6744 =( GEOMETRIC_REPRESENTATION_CONTEXT ( 3 ) GLOBAL_UNCERTAINTY_ASSIGNED_CONTEXT ( ( #30 ) ) GLOBAL_UNIT_ASSIGNED_CONTEXT ( ( #8409, #5681, #762 ) ) REPRESENTATION_CONTEXT ( 'NONE', 'WORKASPACE' ) );
#6745 = CARTESIAN_POINT ( 'NONE',  ( -14.19078112930533209, 29.75000000000008882, 79.50000000000000000 ) ) ;
#6746 = ORIENTED_EDGE ( 'NONE', *, *, #1138, .F. ) ;
#6747 = DIRECTION ( 'NONE',  ( 0.000000000000000000, 0.000000000000000000, 1.000000000000000000 ) ) ;
#6748 = CYLINDRICAL_SURFACE ( 'NONE', #11872, 2.099999999999993427 ) ;
#6749 = VERTEX_POINT ( 'NONE', #9333 ) ;
#6750 = FACE_OUTER_BOUND ( 'NONE', #2923, .T. ) ;
#6751 = CARTESIAN_POINT ( 'NONE',  ( 4.999999999999997335, 0.000000000000000000, 0.000000000000000000 ) ) ;
#6752 = DIRECTION ( 'NONE',  ( 0.000000000000000000, 0.000000000000000000, 1.000000000000000000 ) ) ;
#6753 = DIRECTION ( 'NONE',  ( -0.000000000000000000, -1.000000000000000000, -0.000000000000000000 ) ) ;
#6754 = CARTESIAN_POINT ( 'NONE',  ( 2.979367062500000163, 114.1562499993171969, 0.000000000000000000 ) ) ;
#6755 = CARTESIAN_POINT ( 'NONE',  ( -1.121994411437819084, 112.8749999986344079, 2.708734124999999882 ) ) ;
#6756 =( LENGTH_UNIT ( ) NAMED_UNIT ( * ) SI_UNIT ( .MILLI., .METRE. ) );
#6757 = VERTEX_POINT ( 'NONE', #9395 ) ;
#6758 = CARTESIAN_POINT ( 'NONE',  ( 9.514435292357342533, 40.51730218646115844, 74.39473334479674804 ) ) ;
#6759 = ORIENTED_EDGE ( 'NONE', *, *, #8017, .F. ) ;
#6760 = ADVANCED_FACE ( 'NONE', ( #2800 ), #8523, .T. ) ;
#6761 = PLANE ( 'NONE',  #242 ) ;
#6762 = VECTOR ( 'NONE', #6808, 1000.000000000000114 ) ;
#6763 = LINE ( 'NONE', #147, #1780 ) ;
#6764 = DIRECTION ( 'NONE',  ( 0.000000000000000000, 1.000000000000000000, 0.000000000000000000 ) ) ;
#6765 = CARTESIAN_POINT ( 'NONE',  ( -2.708734125000000770, 110.8749999986343937, -1.121994411437818639 ) ) ;
#6766 = ORIENTED_EDGE ( 'NONE', *, *, #1907, .T. ) ;
#6767 = ORIENTED_EDGE ( 'NONE', *, *, #3540, .F. ) ;
#6768 = AXIS2_PLACEMENT_3D ( 'NONE', #5889, #9670, #382 ) ;
#6769 = APPLICATION_CONTEXT ( 'automotive_design' ) ;
#6770 = ADVANCED_FACE ( 'NONE', ( #755 ), #3554, .F. ) ;
#6771 = EDGE_CURVE ( 'NONE', #5735, #1734, #689, .T. ) ;
#6772 = CARTESIAN_POINT ( 'NONE',  ( 71.69656859387023928, 44.65045859775734982, -22.14271594285822431 ) ) ;
#6773 = EDGE_CURVE ( 'NONE', #10965, #5376, #858, .T. ) ;
#6774 = CARTESIAN_POINT ( 'NONE',  ( 1.377727649040772626E-14, 345.0000000000000568, -110.0000000000000284 ) ) ;
#6775 = PLANE ( 'NONE',  #1027 ) ;
#6776 = CARTESIAN_POINT ( 'NONE',  ( 2.298097038856278918, 112.8750000000000000, -2.298097038856279806 ) ) ;
#6777 = CARTESIAN_POINT ( 'NONE',  ( 71.54748821555645577, 15.63447443924222569, -22.64388168111003807 ) ) ;
#6778 = ORIENTED_EDGE ( 'NONE', *, *, #6726, .T. ) ;
#6779 = VECTOR ( 'NONE', #11345, 1000.000000000000000 ) ;
#6780 = DIRECTION ( 'NONE',  ( 0.000000000000000000, 1.000000000000000000, 0.000000000000000000 ) ) ;
#6781 = VECTOR ( 'NONE', #2963, 1000.000000000000000 ) ;
#6782 = DIRECTION ( 'NONE',  ( 0.000000000000000000, 1.000000000000000000, 0.000000000000000000 ) ) ;
#6783 = ORIENTED_EDGE ( 'NONE', *, *, #2875, .F. ) ;
#6784 = CARTESIAN_POINT ( 'NONE',  ( -5.970153145843347347E-16, 113.6249999972688158, -3.250000000000000444 ) ) ;
#6785 = EDGE_CURVE ( 'NONE', #357, #10533, #9518, .T. ) ;
#6786 =( BOUNDED_CURVE ( )  B_SPLINE_CURVE ( 3, ( #10683, #9735, #270, #5832 ),
 .UNSPECIFIED., .F., .F. ) 
 B_SPLINE_CURVE_WITH_KNOTS ( ( 4, 4 ),
 ( 0.000000000000000000, 1.570796326794896558 ),
 .UNSPECIFIED. ) 
 CURVE ( )  GEOMETRIC_REPRESENTATION_ITEM ( )  RATIONAL_B_SPLINE_CURVE ( ( 1.000000000000000000, 0.8047378541243649375, 0.8047378541243649375, 1.000000000000000000 ) ) 
 REPRESENTATION_ITEM ( '' )  );
#6787 = VECTOR ( 'NONE', #4028, 1000.000000000000000 ) ;
#6788 = EDGE_CURVE ( 'NONE', #10214, #4082, #2448, .T. ) ;
#6789 = EDGE_CURVE ( 'NONE', #2446, #3440, #1654, .T. ) ;
#6790 = ORIENTED_EDGE ( 'NONE', *, *, #5572, .F. ) ;
#6791 = CYLINDRICAL_SURFACE ( 'NONE', #10704, 4.250000000000000000 ) ;
#6792 = DIRECTION ( 'NONE',  ( -0.7071067811865513475, -0.7071067811865437980, -0.000000000000000000 ) ) ;
#6793 = ORIENTED_EDGE ( 'NONE', *, *, #10512, .T. ) ;
#6794 = CARTESIAN_POINT ( 'NONE',  ( 34.73110591274434000, 77.00000000000000000, -8.660254037844445918 ) ) ;
#6795 = FACE_OUTER_BOUND ( 'NONE', #9652, .T. ) ;
#6796 = ORIENTED_EDGE ( 'NONE', *, *, #7250, .T. ) ;
#6797 = AXIS2_PLACEMENT_3D ( 'NONE', #10215, #5497, #4847 ) ;
#6798 = APPLICATION_PROTOCOL_DEFINITION ( 'draft international standard', 'automotive_design', 1998, #1041 ) ;
#6799 = DIRECTION ( 'NONE',  ( -0.8660254037844385966, 0.5000000000000000000, 0.000000000000000000 ) ) ;
#6800 = VECTOR ( 'NONE', #4308, 1000.000000000000000 ) ;
#6801 = CARTESIAN_POINT ( 'NONE',  ( 0.000000000000000000, 65.00000000000000000, 0.000000000000000000 ) ) ;
#6802 = VERTEX_POINT ( 'NONE', #8584 ) ;
#6803 = CARTESIAN_POINT ( 'NONE',  ( 1.915364268218908927, 112.1874999986344079, -1.915364268218909816 ) ) ;
#6804 = CARTESIAN_POINT ( 'NONE',  ( 2.298097038856279806, 110.9999999972688158, 2.298097038856279806 ) ) ;
#6805 = VECTOR ( 'NONE', #1475, 1000.000000000000000 ) ;
#6806 = AXIS2_PLACEMENT_3D ( 'NONE', #6736, #4869, #11418 ) ;
#6807 = ORIENTED_EDGE ( 'NONE', *, *, #3057, .T. ) ;
#6808 = DIRECTION ( 'NONE',  ( -0.4999999999999942268, 0.8660254037844419273, 0.000000000000000000 ) ) ;
#6809 = DIRECTION ( 'NONE',  ( 6.938893903907222067E-15, 1.000000000000000000, 0.000000000000000000 ) ) ;
#6810 = ORIENTED_EDGE ( 'NONE', *, *, #8299, .F. ) ;
#6811 = FACE_OUTER_BOUND ( 'NONE', #5082, .T. ) ;
#6812 = DIRECTION ( 'NONE',  ( 0.000000000000000000, 0.000000000000000000, 1.000000000000000000 ) ) ;
#6813 = EDGE_LOOP ( 'NONE', ( #9550, #6767 ) ) ;
#6814 = DIRECTION ( 'NONE',  ( -0.000000000000000000, -0.000000000000000000, 1.000000000000000000 ) ) ;
#6815 = DIRECTION ( 'NONE',  ( -1.000000000000000000, 0.000000000000000000, -0.000000000000000000 ) ) ;
#6816 = CARTESIAN_POINT ( 'NONE',  ( 0.000000000000000000, 122.0000000000000000, 17.00000000000000000 ) ) ;
#6817 = FACE_OUTER_BOUND ( 'NONE', #2204, .T. ) ;
#6818 = DIRECTION ( 'NONE',  ( 0.000000000000000000, 0.000000000000000000, 1.000000000000000000 ) ) ;
#6819 = ADVANCED_FACE ( 'NONE', ( #5982 ), #7897, .F. ) ;
#6820 = CARTESIAN_POINT ( 'NONE',  ( -2.708734124999999882, 112.9999999986344079, 1.121994411437819084 ) ) ;
#6821 =( NAMED_UNIT ( * ) SI_UNIT ( $, .STERADIAN. ) SOLID_ANGLE_UNIT ( ) );
#6822 = ORIENTED_EDGE ( 'NONE', *, *, #559, .T. ) ;
#6823 = DIRECTION ( 'NONE',  ( 0.000000000000000000, 0.000000000000000000, 1.000000000000000000 ) ) ;
#6824 = CARTESIAN_POINT ( 'NONE',  ( 0.9349062160761316687, 44.87820708871510789, 75.00000000000002842 ) ) ;
#6825 = VECTOR ( 'NONE', #1965, 1000.000000000000114 ) ;
#6826 = VERTEX_POINT ( 'NONE', #2054 ) ;
#6827 = DIRECTION ( 'NONE',  ( 8.881784197001252323E-16, 0.000000000000000000, 1.000000000000000000 ) ) ;
#6828 = CARTESIAN_POINT ( 'NONE',  ( -5.970153145843347347E-16, 112.6249999972688158, -3.250000000000000444 ) ) ;
#6829 = CARTESIAN_POINT ( 'NONE',  ( -6.000000000000000000, 62.00000000000000000, 69.74238309665079782 ) ) ;
#6830 = DIRECTION ( 'NONE',  ( 0.000000000000000000, 0.000000000000000000, 1.000000000000000000 ) ) ;
#6831 = ORIENTED_EDGE ( 'NONE', *, *, #10610, .T. ) ;
#6832 = EDGE_LOOP ( 'NONE', ( #4987, #4858 ) ) ;
#6833 =( NAMED_UNIT ( * ) PLANE_ANGLE_UNIT ( ) SI_UNIT ( $, .RADIAN. ) );
#6834 = ORIENTED_EDGE ( 'NONE', *, *, #7572, .F. ) ;
#6835 = CIRCLE ( 'NONE', #1069, 24.99999999999999645 ) ;
#6836 = EDGE_CURVE ( 'NONE', #10533, #8585, #3986, .T. ) ;
#6837 = EDGE_CURVE ( 'NONE', #632, #4906, #237, .T. ) ;
#6838 = LINE ( 'NONE', #4971, #2254 ) ;
#6839 = DIRECTION ( 'NONE',  ( 0.000000000000000000, 0.000000000000000000, 1.000000000000000000 ) ) ;
#6840 = ORIENTED_EDGE ( 'NONE', *, *, #2975, .T. ) ;
#6841 = DIRECTION ( 'NONE',  ( 1.000000000000000000, 0.000000000000000000, 0.000000000000000000 ) ) ;
#6842 = CARTESIAN_POINT ( 'NONE',  ( 71.59683363033870762, 15.53272889911889543, -22.47949853503603990 ) ) ;
#6843 = VERTEX_POINT ( 'NONE', #9584 ) ;
#6844 = CARTESIAN_POINT ( 'NONE',  ( -32.15778161310143446, 87.00000000000000000, -8.660254037844435260 ) ) ;
#6845 = DIRECTION ( 'NONE',  ( 0.000000000000000000, -0.4999999999999993339, 0.8660254037844390407 ) ) ;
#6846 = ORIENTED_EDGE ( 'NONE', *, *, #11505, .T. ) ;
#6847 = CARTESIAN_POINT ( 'NONE',  ( -1.346194077712542736, 113.5624999972688016, -3.250000000000017764 ) ) ;
#6848 = EDGE_CURVE ( 'NONE', #5951, #434, #47, .T. ) ;
#6849 = ADVANCED_FACE ( 'NONE', ( #10468 ), #6915, .F. ) ;
#6850 = CIRCLE ( 'NONE', #1479, 2.041999999999999815 ) ;
#6851 = CIRCLE ( 'NONE', #12237, 5.000000000000004441 ) ;
#6852 = ORIENTED_EDGE ( 'NONE', *, *, #10951, .F. ) ;
#6853 = DIRECTION ( 'NONE',  ( 0.8660254037844331565, -0.5000000000000095479, 0.000000000000000000 ) ) ;
#6854 = FACE_OUTER_BOUND ( 'NONE', #5425, .T. ) ;
#6855 = ORIENTED_EDGE ( 'NONE', *, *, #11291, .T. ) ;
#6856 = DIRECTION ( 'NONE',  ( 0.000000000000000000, -1.000000000000000000, 0.000000000000000000 ) ) ;
#6857 = LINE ( 'NONE', #9587, #11277 ) ;
#6858 = ORIENTED_EDGE ( 'NONE', *, *, #3357, .T. ) ;
#6859 = SHAPE_DEFINITION_REPRESENTATION ( #3790, #9674 ) ;
#6860 = CARTESIAN_POINT ( 'NONE',  ( 25.00000000000000355, 445.0000000000000568, -88.00000000000000000 ) ) ;
#6861 = FACE_OUTER_BOUND ( 'NONE', #11396, .T. ) ;
#6862 = ADVANCED_FACE ( 'NONE', ( #6854 ), #8831, .F. ) ;
#6863 = EDGE_CURVE ( 'NONE', #6075, #10718, #11536, .T. ) ;
#6864 = ORIENTED_EDGE ( 'NONE', *, *, #2239, .T. ) ;
#6865 = CARTESIAN_POINT ( 'NONE',  ( 1.121994411437819528, 111.1249999986343937, -2.708734124999999882 ) ) ;
#6866 = CARTESIAN_POINT ( 'NONE',  ( -1.346194077712559389, 112.1874999972688016, 3.250000000000000444 ) ) ;
#6867 = ORIENTED_EDGE ( 'NONE', *, *, #1080, .T. ) ;
#6868 = CARTESIAN_POINT ( 'NONE',  ( 0.000000000000000000, 5.051668046482832750E-16, -4.000000000000000000 ) ) ;
#6869 = CARTESIAN_POINT ( 'NONE',  ( 0.000000000000000000, 115.0000000000000000, 0.000000000000000000 ) ) ;
#6870 = CIRCLE ( 'NONE', #5682, 110.0000000000000284 ) ;
#6871 = EDGE_LOOP ( 'NONE', ( #8229, #7361, #5353, #515, #10912, #4593, #1989, #121 ) ) ;
#6872 = VECTOR ( 'NONE', #6192, 1000.000000000000000 ) ;
#6873 = DIRECTION ( 'NONE',  ( 0.000000000000000000, 1.000000000000000000, 0.000000000000000000 ) ) ;
#6874 = CARTESIAN_POINT ( 'NONE',  ( 9.942549119892305498, 36.71650635094628967, 79.50000000000000000 ) ) ;
#6875 = EDGE_LOOP ( 'NONE', ( #2824, #5816, #1772, #10024 ) ) ;
#6876 = DIRECTION ( 'NONE',  ( -0.000000000000000000, -1.000000000000000000, -0.000000000000000000 ) ) ;
#6877 = CARTESIAN_POINT ( 'NONE',  ( -97.61745645432043261, 275.0000000000000000, 78.07581056504542971 ) ) ;
#6878 = LINE ( 'NONE', #10793, #11773 ) ;
#6879 = DIRECTION ( 'NONE',  ( -1.000000000000000000, -0.000000000000000000, -0.000000000000000000 ) ) ;
#6880 = CARTESIAN_POINT ( 'NONE',  ( 0.000000000000000000, 110.0000000000000000, 0.000000000000000000 ) ) ;
#6881 = CARTESIAN_POINT ( 'NONE',  ( 1.915364268218908705, 114.4374999986344079, -1.915364268218909594 ) ) ;
#6882 = AXIS2_PLACEMENT_3D ( 'NONE', #734, #4528, #12141 ) ;
#6883 = ORIENTED_EDGE ( 'NONE', *, *, #3454, .F. ) ;
#6884 = VERTEX_POINT ( 'NONE', #5737 ) ;
#6885 = PRODUCT_DEFINITION_SHAPE ( 'NONE', 'NONE',  #12356 ) ;
#6886 = ADVANCED_FACE ( 'NONE', ( #2861 ), #8613, .T. ) ;
#6887 = CARTESIAN_POINT ( 'NONE',  ( 21.00000000000000355, 2.789133085058097101E-16, -2.055000000000000160 ) ) ;
#6888 = EDGE_CURVE ( 'NONE', #108, #1518, #5920, .T. ) ;
#6889 = CARTESIAN_POINT ( 'NONE',  ( 2.500000000000000000, -1.768423874527825568, -1.020999999999998575 ) ) ;
#6890 = ORIENTED_EDGE ( 'NONE', *, *, #4636, .T. ) ;
#6891 = DIRECTION ( 'NONE',  ( 0.000000000000000000, 1.000000000000000000, 0.000000000000000000 ) ) ;
#6892 = VECTOR ( 'NONE', #3835, 1000.000000000000000 ) ;
#6893 = DIRECTION ( 'NONE',  ( 0.000000000000000000, 0.000000000000000000, -1.000000000000000000 ) ) ;
#6894 = VECTOR ( 'NONE', #9935, 1000.000000000000000 ) ;
#6895 = CARTESIAN_POINT ( 'NONE',  ( -25.00000000000000000, 345.0000000000000568, -24.99999999999998934 ) ) ;
#6896 = DIRECTION ( 'NONE',  ( 0.5000000000000066613, 0.8660254037844347108, 0.000000000000000000 ) ) ;
#6897 = EDGE_CURVE ( 'NONE', #9831, #4212, #6714, .T. ) ;
#6898 = AXIS2_PLACEMENT_3D ( 'NONE', #3364, #4164, #617 ) ;
#6899 = VERTEX_POINT ( 'NONE', #4408 ) ;
#6900 =( NAMED_UNIT ( * ) SI_UNIT ( $, .STERADIAN. ) SOLID_ANGLE_UNIT ( ) );
#6901 = CIRCLE ( 'NONE', #7883, 10.00000000000000178 ) ;
#6902 = SURFACE_STYLE_FILL_AREA ( #8813 ) ;
#6903 = CARTESIAN_POINT ( 'NONE',  ( 1.285879139104721264E-14, 275.0000000000000000, -105.0000000000000426 ) ) ;
#6904 = DIRECTION ( 'NONE',  ( 0.000000000000000000, -0.4999999999999989453, 0.8660254037844391517 ) ) ;
#6905 = ORIENTED_EDGE ( 'NONE', *, *, #11915, .F. ) ;
#6906 = CARTESIAN_POINT ( 'NONE',  ( 0.000000000000000000, 75.00000000000001421, 0.000000000000000000 ) ) ;
#6907 = CARTESIAN_POINT ( 'NONE',  ( 74.98782882127120786, 16.91249280870930605, -23.93624459205407362 ) ) ;
#6908 = DIRECTION ( 'NONE',  ( -0.000000000000000000, 1.000000000000000000, -0.000000000000000000 ) ) ;
#6909 = CARTESIAN_POINT ( 'NONE',  ( 10.06754911989233392, 36.50000000000012079, 80.00000000000000000 ) ) ;
#6910 = VERTEX_POINT ( 'NONE', #2483 ) ;
#6911 = DIRECTION ( 'NONE',  ( -1.000000000000000000, -0.000000000000000000, -0.000000000000000000 ) ) ;
#6912 = VECTOR ( 'NONE', #10548, 1000.000000000000000 ) ;
#6913 = VERTEX_POINT ( 'NONE', #10016 ) ;
#6914 = CYLINDRICAL_SURFACE ( 'NONE', #10314, 30.00000000000000711 ) ;
#6915 = PLANE ( 'NONE',  #456 ) ;
#6916 = VERTEX_POINT ( 'NONE', #11715 ) ;
#6917 = DIRECTION ( 'NONE',  ( -0.000000000000000000, -1.000000000000000000, -0.000000000000000000 ) ) ;
#6918 = CARTESIAN_POINT ( 'NONE',  ( 0.000000000000000000, 290.0000000000000568, 0.000000000000000000 ) ) ;
#6919 = ORIENTED_EDGE ( 'NONE', *, *, #3661, .T. ) ;
#6920 = EDGE_CURVE ( 'NONE', #10198, #1420, #11964, .T. ) ;
#6921 = CARTESIAN_POINT ( 'NONE',  ( 5.525725221640672480, 41.13333024919784719, 80.00000000000000000 ) ) ;
#6922 = CARTESIAN_POINT ( 'NONE',  ( 30.00000000000004263, 65.00000000000000000, -63.24555320336758513 ) ) ;
#6923 = EDGE_LOOP ( 'NONE', ( #3320, #2302, #4120, #4015 ) ) ;
#6924 = CARTESIAN_POINT ( 'NONE',  ( 1.915364268218909594, 112.4374999986344079, 1.915364268218909594 ) ) ;
#6925 = CARTESIAN_POINT ( 'NONE',  ( 2.298097038856278918, 113.7499999972688158, -2.298097038856279806 ) ) ;
#6926 = ORIENTED_EDGE ( 'NONE', *, *, #3164, .F. ) ;
#6927 = EDGE_CURVE ( 'NONE', #10169, #11869, #2645, .T. ) ;
#6928 = FACE_OUTER_BOUND ( 'NONE', #5018, .T. ) ;
#6929 = DIRECTION ( 'NONE',  ( 1.000000000000000000, -0.000000000000000000, 0.000000000000000000 ) ) ;
#6930 = EDGE_CURVE ( 'NONE', #10079, #3797, #4234, .T. ) ;
#6931 = ORIENTED_EDGE ( 'NONE', *, *, #1333, .T. ) ;
#6932 = LINE ( 'NONE', #2190, #1819 ) ;
#6933 = CARTESIAN_POINT ( 'NONE',  ( 69.64721689463594601, 17.41064966062540620, 27.82591776719579713 ) ) ;
#6934 = VECTOR ( 'NONE', #2987, 1000.000000000000000 ) ;
#6935 = EDGE_LOOP ( 'NONE', ( #3559, #9625, #10422, #3153 ) ) ;
#6936 = CYLINDRICAL_SURFACE ( 'NONE', #5486, 9.999999999999998224 ) ;
#6937 = CARTESIAN_POINT ( 'NONE',  ( -27.30107202361637775, 86.87046582918780757, -12.43589427268144831 ) ) ;
#6938 = CARTESIAN_POINT ( 'NONE',  ( 25.00000000000000355, 445.0000000000000568, -105.0000000000000000 ) ) ;
#6939 = ORIENTED_EDGE ( 'NONE', *, *, #8037, .F. ) ;
#6940 = DIRECTION ( 'NONE',  ( 0.5000000000000066613, 0.8660254037844347108, 0.000000000000000000 ) ) ;
#6941 = CARTESIAN_POINT ( 'NONE',  ( 25.00000000000000000, 570.2996408614167194, -29.99999999999998934 ) ) ;
#6942 = EDGE_CURVE ( 'NONE', #2274, #12042, #546, .T. ) ;
#6943 = AXIS2_PLACEMENT_3D ( 'NONE', #9489, #2588, #6577 ) ;
#6944 = ORIENTED_EDGE ( 'NONE', *, *, #8620, .T. ) ;
#6945 = CARTESIAN_POINT ( 'NONE',  ( 77.29025109341738187, 45.00000000000009237, -20.32807234521402151 ) ) ;
#6946 = ORIENTED_EDGE ( 'NONE', *, *, #5259, .T. ) ;
#6947 = DIRECTION ( 'NONE',  ( -0.000000000000000000, -0.000000000000000000, 1.000000000000000000 ) ) ;
#6948 = CARTESIAN_POINT ( 'NONE',  ( 8.485645551905516726, 41.47111475299955430, 74.51923978935600701 ) ) ;
#6949 = ORIENTED_EDGE ( 'NONE', *, *, #538, .F. ) ;
#6950 = DIRECTION ( 'NONE',  ( 0.000000000000000000, 1.000000000000000000, 0.000000000000000000 ) ) ;
#6951 = DIRECTION ( 'NONE',  ( 0.000000000000000000, 0.000000000000000000, -1.000000000000000000 ) ) ;
#6952 = CARTESIAN_POINT ( 'NONE',  ( -7.907287480251413925, 18.86666975080236597, 80.00000000000000000 ) ) ;
#6953 = EDGE_CURVE ( 'NONE', #11346, #4808, #486, .T. ) ;
#6954 = EDGE_LOOP ( 'NONE', ( #11066, #6890, #9687, #8176, #2821, #9616, #5432, #4540, #4485 ) ) ;
#6955 = EDGE_CURVE ( 'NONE', #5680, #693, #8019, .T. ) ;
#6956 = AXIS2_PLACEMENT_3D ( 'NONE', #7279, #9124, #4825 ) ;
#6957 = VECTOR ( 'NONE', #7252, 1000.000000000000000 ) ;
#6958 = DIRECTION ( 'NONE',  ( 0.000000000000000000, 1.000000000000000000, 0.000000000000000000 ) ) ;
#6959 = CARTESIAN_POINT ( 'NONE',  ( 0.000000000000000000, 87.00000000000000000, 24.99999999999999645 ) ) ;
#6960 = FACE_OUTER_BOUND ( 'NONE', #4975, .T. ) ;
#6961 =( NAMED_UNIT ( * ) SI_UNIT ( $, .STERADIAN. ) SOLID_ANGLE_UNIT ( ) );
#6962 = DIRECTION ( 'NONE',  ( -0.000000000000000000, -1.000000000000000000, -0.000000000000000000 ) ) ;
#6963 = LINE ( 'NONE', #8885, #2672 ) ;
#6964 = CARTESIAN_POINT ( 'NONE',  ( 1.915364268218908927, 113.1874999986344079, -1.915364268218909816 ) ) ;
#6965 = CIRCLE ( 'NONE', #4985, 72.00000000000002842 ) ;
#6966 = ORIENTED_EDGE ( 'NONE', *, *, #10414, .F. ) ;
#6967 = DIRECTION ( 'NONE',  ( 0.000000000000000000, 0.000000000000000000, -1.000000000000000000 ) ) ;
#6968 = ADVANCED_FACE ( 'NONE', ( #10773 ), #2041, .F. ) ;
#6969 = VECTOR ( 'NONE', #5873, 1000.000000000000000 ) ;
#6970 = ORIENTED_EDGE ( 'NONE', *, *, #10307, .T. ) ;
#6971 = CIRCLE ( 'NONE', #9551, 40.00000000000000000 ) ;
#6972 = DIRECTION ( 'NONE',  ( -0.000000000000000000, -0.000000000000000000, 1.000000000000000000 ) ) ;
#6973 = VERTEX_POINT ( 'NONE', #9827 ) ;
#6974 = CARTESIAN_POINT ( 'NONE',  ( -0.9407811293052825707, 17.00000000000008882, 79.50000000000000000 ) ) ;
#6975 = LINE ( 'NONE', #9645, #4498 ) ;
#6976 = EDGE_LOOP ( 'NONE', ( #4689, #6225, #8701, #5169 ) ) ;
#6977 = CARTESIAN_POINT ( 'NONE',  ( -45.35898384862240107, 85.26794919243110371, -9.660254037844429931 ) ) ;
#6978 = PLANE ( 'NONE',  #5213 ) ;
#6979 = ORIENTED_EDGE ( 'NONE', *, *, #9336, .F. ) ;
#6980 = CARTESIAN_POINT ( 'NONE',  ( -1.915364268218909150, 113.6874999986344079, 1.915364268218909594 ) ) ;
#6981 = CIRCLE ( 'NONE', #4790, 5.000000000000000888 ) ;
#6982 = EDGE_CURVE ( 'NONE', #5298, #2436, #10895, .T. ) ;
#6983 = ADVANCED_FACE ( 'NONE', ( #2295 ), #7220, .T. ) ;
#6984 = EDGE_CURVE ( 'NONE', #7967, #3932, #6835, .T. ) ;
#6985 = ORIENTED_EDGE ( 'NONE', *, *, #761, .T. ) ;
#6986 = CARTESIAN_POINT ( 'NONE',  ( 28.61611180472260330, 87.72948999988453522, 9.923767781257849308 ) ) ;
#6987 = LINE ( 'NONE', #9718, #5081 ) ;
#6988 = ORIENTED_EDGE ( 'NONE', *, *, #6627, .T. ) ;
#6989 = DIRECTION ( 'NONE',  ( 0.000000000000000000, 0.000000000000000000, 1.000000000000000000 ) ) ;
#6990 = FACE_OUTER_BOUND ( 'NONE', #10466, .T. ) ;
#6991 = AXIS2_PLACEMENT_3D ( 'NONE', #5137, #380, #6248 ) ;
#6992 = ORIENTED_EDGE ( 'NONE', *, *, #5971, .T. ) ;
#6993 = PLANE ( 'NONE',  #10849 ) ;
#6994 = DIRECTION ( 'NONE',  ( -0.000000000000000000, 1.000000000000000000, -0.000000000000000000 ) ) ;
#6995 = CARTESIAN_POINT ( 'NONE',  ( 5.000000000000002665, 0.000000000000000000, -2.700000000000000622 ) ) ;
#6996 = ORIENTED_EDGE ( 'NONE', *, *, #2689, .T. ) ;
#6997 = DIRECTION ( 'NONE',  ( 1.000000000000000000, 0.000000000000000000, 0.000000000000000000 ) ) ;
#6998 = AXIS2_PLACEMENT_3D ( 'NONE', #7768, #1689, #1044 ) ;
#6999 = CARTESIAN_POINT ( 'NONE',  ( 72.13972991038781402, 14.87494484084908386, 20.57104709750045402 ) ) ;
#7000 = CIRCLE ( 'NONE', #8581, 30.00000000000000355 ) ;
#7001 = EDGE_CURVE ( 'NONE', #861, #9973, #4161, .T. ) ;
#7002 = ORIENTED_EDGE ( 'NONE', *, *, #12198, .F. ) ;
#7003 = CARTESIAN_POINT ( 'NONE',  ( 74.62554477486000337, 17.62767568092783321, 24.41456952963950755 ) ) ;
#7004 = CARTESIAN_POINT ( 'NONE',  ( 76.19556706709904859, 44.50529433006728652, -22.19251267860074961 ) ) ;
#7005 = EDGE_LOOP ( 'NONE', ( #9464, #2308, #9711, #5355 ) ) ;
#7006 = ADVANCED_FACE ( 'NONE', ( #9010 ), #8082, .T. ) ;
#7007 = PRODUCT_DEFINITION_CONTEXT ( 'detailed design', #2548, 'design' ) ;
#7008 = CARTESIAN_POINT ( 'NONE',  ( 1.347111479062088996E-14, 340.0000000000000000, 110.0000000000000284 ) ) ;
#7009 = CARTESIAN_POINT ( 'NONE',  ( 70.79098555864042908, 40.00000000000009237, 25.00000000000000000 ) ) ;
#7010 = ORIENTED_EDGE ( 'NONE', *, *, #681, .F. ) ;
#7011 = DIRECTION ( 'NONE',  ( -0.000000000000000000, -1.000000000000000000, -0.000000000000000000 ) ) ;
#7012 = DIRECTION ( 'NONE',  ( 0.000000000000000000, -0.000000000000000000, 1.000000000000000000 ) ) ;
#7013 = LINE ( 'NONE', #6022, #1332 ) ;
#7014 = CARTESIAN_POINT ( 'NONE',  ( 0.000000000000000000, 65.00000000000000000, 0.000000000000000000 ) ) ;
#7015 = EDGE_CURVE ( 'NONE', #8096, #11474, #3361, .T. ) ;
#7016 = EDGE_CURVE ( 'NONE', #11371, #10583, #358, .T. ) ;
#7017 = ORIENTED_EDGE ( 'NONE', *, *, #4354, .T. ) ;
#7018 = VERTEX_POINT ( 'NONE', #928 ) ;
#7019 = CIRCLE ( 'NONE', #10194, 5.000000000000001776 ) ;
#7020 =( LENGTH_UNIT ( ) NAMED_UNIT ( * ) SI_UNIT ( .MILLI., .METRE. ) );
#7021 = DIRECTION ( 'NONE',  ( 0.000000000000000000, 0.000000000000000000, 1.000000000000000000 ) ) ;
#7022 = DIRECTION ( 'NONE',  ( -1.000000000000000000, -0.000000000000000000, -0.000000000000000000 ) ) ;
#7023 = DIRECTION ( 'NONE',  ( 0.000000000000000000, -0.4999999999999993339, 0.8660254037844390407 ) ) ;
#7024 = DIRECTION ( 'NONE',  ( 1.000000000000000000, 0.000000000000000000, -0.000000000000000000 ) ) ;
#7025 = CARTESIAN_POINT ( 'NONE',  ( -2.708734125000000770, 112.8749999986344079, -1.121994411437818639 ) ) ;
#7026 = VECTOR ( 'NONE', #7483, 1000.000000000000000 ) ;
#7027 = ORIENTED_EDGE ( 'NONE', *, *, #9513, .F. ) ;
#7028 = DIRECTION ( 'NONE',  ( -1.000000000000000000, -0.000000000000000000, -0.000000000000000000 ) ) ;
#7029 = ORIENTED_EDGE ( 'NONE', *, *, #10585, .F. ) ;
#7030 = CIRCLE ( 'NONE', #3852, 12.99999999999999822 ) ;
#7031 = DIRECTION ( 'NONE',  ( -0.4999999999999985012, -0.8660254037844394848, 0.000000000000000000 ) ) ;
#7032 = ORIENTED_EDGE ( 'NONE', *, *, #10384, .T. ) ;
#7033 = DIRECTION ( 'NONE',  ( 1.224646799147349509E-16, 0.000000000000000000, -1.000000000000000000 ) ) ;
#7034 = EDGE_CURVE ( 'NONE', #2259, #1429, #2604, .T. ) ;
#7035 = LINE ( 'NONE', #425, #7489 ) ;
#7036 = ORIENTED_EDGE ( 'NONE', *, *, #7330, .T. ) ;
#7037 = CARTESIAN_POINT ( 'NONE',  ( -20.00000000000000355, 7.965803112215716020, -57.08203932499370836 ) ) ;
#7038 =( BOUNDED_SURFACE ( )  B_SPLINE_SURFACE ( 3, 2, ( 
 ( #6305, #10089, #1690 ),
 ( #12109, #11298, #6366 ),
 ( #7428, #820, #2559 ),
 ( #11230, #5498, #759 ) ),
 .UNSPECIFIED., .F., .F., .F. ) 
 B_SPLINE_SURFACE_WITH_KNOTS ( ( 4, 4 ),
 ( 3, 3 ),
 ( 1.665911834627059607, 1.695449464845517618 ),
 ( 0.2468956587999593388, 1.000000000000000000 ),
 .UNSPECIFIED. ) 
 GEOMETRIC_REPRESENTATION_ITEM ( )  RATIONAL_B_SPLINE_SURFACE ( (
 ( 0.8800340755151767613, 0.7570513692546891882, 1.000000000000000000),
 ( 0.8788691223080344894, 0.7546921677749939272, 1.000000000000000000),
 ( 0.8776977286441711712, 0.7523199234237630817, 1.000000000000000000),
 ( 0.8765201392483088494, 0.7499351318045301973, 1.000000000000000000) ) ) 
 REPRESENTATION_ITEM ( '' )  SURFACE ( )  );
#7039 = CARTESIAN_POINT ( 'NONE',  ( 100.7495955565343451, 275.0000000000000000, 29.57226733266770680 ) ) ;
#7040 = EDGE_CURVE ( 'NONE', #11519, #9781, #4596, .T. ) ;
#7041 = ORIENTED_EDGE ( 'NONE', *, *, #10028, .F. ) ;
#7042 = CARTESIAN_POINT ( 'NONE',  ( 69.85318522031718658, 44.10340835627246037, -27.30472166927799194 ) ) ;
#7043 = CIRCLE ( 'NONE', #10822, 15.00000000000000000 ) ;
#7044 = AXIS2_PLACEMENT_3D ( 'NONE', #9153, #633, #11736 ) ;
#7045 = ORIENTED_EDGE ( 'NONE', *, *, #10672, .F. ) ;
#7046 = EDGE_LOOP ( 'NONE', ( #6524, #1196, #10982, #2959 ) ) ;
#7047 = CARTESIAN_POINT ( 'NONE',  ( 2.708734125000000326, 114.3124999986344079, 0.000000000000000000 ) ) ;
#7048 = DIRECTION ( 'NONE',  ( 0.000000000000000000, 0.000000000000000000, 1.000000000000000000 ) ) ;
#7049 = EDGE_LOOP ( 'NONE', ( #9301, #7294, #6704, #5835, #12349, #3556, #12113, #8862, #4942, #5260 ) ) ;
#7050 = DIRECTION ( 'NONE',  ( 0.000000000000000000, 0.000000000000000000, 1.000000000000000000 ) ) ;
#7051 = DIRECTION ( 'NONE',  ( -1.000000000000000000, 0.000000000000000000, 0.000000000000000000 ) ) ;
#7052 = EDGE_CURVE ( 'NONE', #3002, #9892, #2661, .T. ) ;
#7053 = ORIENTED_EDGE ( 'NONE', *, *, #11746, .F. ) ;
#7054 = AXIS2_PLACEMENT_3D ( 'NONE', #7620, #11249, #10296 ) ;
#7055 = CARTESIAN_POINT ( 'NONE',  ( 0.000000000000000000, 65.00000000000000000, 0.000000000000000000 ) ) ;
#7056 = AXIS2_PLACEMENT_3D ( 'NONE', #8515, #12337, #9509 ) ;
#7057 = CARTESIAN_POINT ( 'NONE',  ( 20.00000000000000711, 63.00000000000000000, 67.08203932499370126 ) ) ;
#7058 = DIRECTION ( 'NONE',  ( -1.000000000000000000, -0.000000000000000000, 0.000000000000000000 ) ) ;
#7059 = ORIENTED_EDGE ( 'NONE', *, *, #7826, .T. ) ;
#7060 = CARTESIAN_POINT ( 'NONE',  ( -1.440781129305471087, 43.00000000000008527, 79.50000000000000000 ) ) ;
#7061 = CARTESIAN_POINT ( 'NONE',  ( 76.01088325117457600, 15.64455795939924698, 22.47665947743448100 ) ) ;
#7062 = AXIS2_PLACEMENT_3D ( 'NONE', #1488, #1427, #10834 ) ;
#7063 = VECTOR ( 'NONE', #2476, 1000.000000000000000 ) ;
#7064 = ORIENTED_EDGE ( 'NONE', *, *, #9144, .T. ) ;
#7065 = CARTESIAN_POINT ( 'NONE',  ( 72.32495769890020654, 45.16153383718148007, -19.87825060515872266 ) ) ;
#7066 = DIRECTION ( 'NONE',  ( -0.000000000000000000, 1.000000000000000000, -0.000000000000000000 ) ) ;
#7067 = VERTEX_POINT ( 'NONE', #8268 ) ;
#7068 = LINE ( 'NONE', #8923, #5855 ) ;
#7069 = CARTESIAN_POINT ( 'NONE',  ( 70.96239324365633649, 42.26132884148638880, 24.49110472308180064 ) ) ;
#7070 = ORIENTED_EDGE ( 'NONE', *, *, #9714, .F. ) ;
#7071 = CARTESIAN_POINT ( 'NONE',  ( -12.57411137850303540, 36.28349364905398033, 79.50000000000000000 ) ) ;
#7072 = CARTESIAN_POINT ( 'NONE',  ( 1.990051048614449116E-16, 112.1249999972688158, 3.250000000000000444 ) ) ;
#7073 = FACE_OUTER_BOUND ( 'NONE', #7049, .T. ) ;
#7074 = CARTESIAN_POINT ( 'NONE',  ( -2.708734125000000770, 111.8749999986343937, -1.121994411437818639 ) ) ;
#7075 = EDGE_CURVE ( 'NONE', #7972, #7578, #9405, .T. ) ;
#7076 = CIRCLE ( 'NONE', #2499, 5.000000000000000888 ) ;
#7077 = CIRCLE ( 'NONE', #6454, 25.50000000000000000 ) ;
#7078 = ORIENTED_EDGE ( 'NONE', *, *, #8297, .F. ) ;
#7079 = FILL_AREA_STYLE_COLOUR ( '', #10132 ) ;
#7080 = VERTEX_POINT ( 'NONE', #10199 ) ;
#7081 = AXIS2_PLACEMENT_3D ( 'NONE', #8729, #191, #3821 ) ;
#7082 = CARTESIAN_POINT ( 'NONE',  ( 10.10921578655968922, 36.42783121635022781, 80.00000000000000000 ) ) ;
#7083 = EDGE_CURVE ( 'NONE', #3881, #5427, #6534, .T. ) ;
#7084 = EDGE_CURVE ( 'NONE', #3436, #10138, #3251, .T. ) ;
#7085 = DIRECTION ( 'NONE',  ( 0.000000000000000000, 0.000000000000000000, 1.000000000000000000 ) ) ;
#7086 = CARTESIAN_POINT ( 'NONE',  ( -7.907287480251413925, 18.86666975080236597, 79.50000000000000000 ) ) ;
#7087 = AXIS2_PLACEMENT_3D ( 'NONE', #11940, #2523, #944 ) ;
#7088 = CARTESIAN_POINT ( 'NONE',  ( 3.250000000000000444, 114.8749999972688158, 0.000000000000000000 ) ) ;
#7089 = CARTESIAN_POINT ( 'NONE',  ( 31.48070082314331231, 75.91043305631261262, -6.547439342558601716 ) ) ;
#7090 = ITEM_DEFINED_TRANSFORMATION ( 'NONE', 'NONE', #5756,  #1612 ) ;
#7091 = CARTESIAN_POINT ( 'NONE',  ( 72.61843774138908714, 10.00000000000017586, -18.75000000000000000 ) ) ;
#7092 = CARTESIAN_POINT ( 'NONE',  ( 1.121994411437819528, 111.1249999986343937, -2.708734124999999882 ) ) ;
#7093 = CIRCLE ( 'NONE', #112, 25.00000000000000000 ) ;
#7094 = VERTEX_POINT ( 'NONE', #8389 ) ;
#7095 = DIRECTION ( 'NONE',  ( 0.000000000000000000, 1.000000000000000000, 0.000000000000000000 ) ) ;
#7096 = ORIENTED_EDGE ( 'NONE', *, *, #2085, .T. ) ;
#7097 = CARTESIAN_POINT ( 'NONE',  ( 32.21610632498789073, 86.34645847305445443, 9.037576414353038601 ) ) ;
#7098 = VERTEX_POINT ( 'NONE', #7411 ) ;
#7099 = DIRECTION ( 'NONE',  ( 0.000000000000000000, 0.000000000000000000, -1.000000000000000000 ) ) ;
#7100 = CARTESIAN_POINT ( 'NONE',  ( 76.23530124607876246, 15.46574672446569387, -22.12995508525856536 ) ) ;
#7101 = VERTEX_POINT ( 'NONE', #12212 ) ;
#7102 = LINE ( 'NONE', #11721, #11444 ) ;
#7103 = AXIS2_PLACEMENT_3D ( 'NONE', #11500, #962, #3758 ) ;
#7104 = FACE_OUTER_BOUND ( 'NONE', #1676, .T. ) ;
#7105 = VERTEX_POINT ( 'NONE', #7286 ) ;
#7106 = CARTESIAN_POINT ( 'NONE',  ( -2.298097038856279362, 113.3750000000000000, 2.298097038856279806 ) ) ;
#7107 = EDGE_CURVE ( 'NONE', #3955, #4409, #10263, .T. ) ;
#7108 = EDGE_CURVE ( 'NONE', #3272, #2243, #803, .T. ) ;
#7109 = ORIENTED_EDGE ( 'NONE', *, *, #8664, .F. ) ;
#7110 = CARTESIAN_POINT ( 'NONE',  ( 28.14852131675075597, 87.98519278820045031, 10.36665800225805611 ) ) ;
#7111 = ADVANCED_FACE ( 'NONE', ( #743, #12151 ), #3722, .T. ) ;
#7112 = DIRECTION ( 'NONE',  ( 0.000000000000000000, 1.000000000000000000, 0.000000000000000000 ) ) ;
#7113 = VERTEX_POINT ( 'NONE', #10320 ) ;
#7114 = DIRECTION ( 'NONE',  ( 0.000000000000000000, 0.000000000000000000, 1.000000000000000000 ) ) ;
#7115 = CARTESIAN_POINT ( 'NONE',  ( 6.000000000000000000, 62.00000000000000000, 70.00000000000001421 ) ) ;
#7116 = ORIENTED_EDGE ( 'NONE', *, *, #3609, .F. ) ;
#7117 = CARTESIAN_POINT ( 'NONE',  ( 25.00000000000000000, 445.0000000000000568, -29.99999999999998934 ) ) ;
#7118 = CYLINDRICAL_SURFACE ( 'NONE', #9877, 5.000000000000001776 ) ;
#7119 = CARTESIAN_POINT ( 'NONE',  ( 1.836970198721029589E-15, 170.0000000000000000, 15.00000000000000000 ) ) ;
#7120 = ORIENTED_EDGE ( 'NONE', *, *, #2494, .F. ) ;
#7121 = FACE_OUTER_BOUND ( 'NONE', #5084, .T. ) ;
#7122 = CARTESIAN_POINT ( 'NONE',  ( 76.75412411316109740, 15.16378490115497080, 21.27950340534427198 ) ) ;
#7123 = ORIENTED_EDGE ( 'NONE', *, *, #351, .T. ) ;
#7124 = VECTOR ( 'NONE', #7357, 1000.000000000000000 ) ;
#7125 = CARTESIAN_POINT ( 'NONE',  ( 77.11525298301567943, 44.96802867796342440, -20.64974928742854132 ) ) ;
#7126 = CARTESIAN_POINT ( 'NONE',  ( 5.092712519748452848, 41.38333024919784719, 80.00000000000000000 ) ) ;
#7127 = ORIENTED_EDGE ( 'NONE', *, *, #5014, .T. ) ;
#7128 = CARTESIAN_POINT ( 'NONE',  ( 1.346194077712550063, 111.1874999999999858, 3.250000000000008438 ) ) ;
#7129 = CARTESIAN_POINT ( 'NONE',  ( 74.26978800665389713, 41.16139233038059331, 24.86610009102963659 ) ) ;
#7130 = ORIENTED_EDGE ( 'NONE', *, *, #10921, .F. ) ;
#7131 = CARTESIAN_POINT ( 'NONE',  ( 5.164881303379191380, 18.65833641745863147, 80.00000048127353125 ) ) ;
#7132 = DIRECTION ( 'NONE',  ( 0.000000000000000000, 1.000000000000000000, 0.000000000000000000 ) ) ;
#7133 = CYLINDRICAL_SURFACE ( 'NONE', #2714, 105.0000000000000426 ) ;
#7134 = CARTESIAN_POINT ( 'NONE',  ( 2.708734124999999882, 113.2499999986344079, -1.121994411437820416 ) ) ;
#7135 = CIRCLE ( 'NONE', #9110, 105.0000000000000284 ) ;
#7136 = SHAPE_REPRESENTATION ( 'Central Drive Shaft Post', ( #1612 ), #9157 ) ;
#7137 = VERTEX_POINT ( 'NONE', #8450 ) ;
#7138 = EDGE_CURVE ( 'NONE', #6884, #10404, #11088, .T. ) ;
#7139 = UNCERTAINTY_MEASURE_WITH_UNIT (LENGTH_MEASURE( 1.000000000000000082E-05 ), #2285, 'distance_accuracy_value', 'NONE');
#7140 = LINE ( 'NONE', #10059, #1872 ) ;
#7141 = EDGE_CURVE ( 'NONE', #4861, #7589, #6638, .T. ) ;
#7142 = LINE ( 'NONE', #4274, #10911 ) ;
#7143 = DIRECTION ( 'NONE',  ( -0.000000000000000000, -0.000000000000000000, -1.000000000000000000 ) ) ;
#7144 =( GEOMETRIC_REPRESENTATION_CONTEXT ( 3 ) GLOBAL_UNCERTAINTY_ASSIGNED_CONTEXT ( ( #6647 ) ) GLOBAL_UNIT_ASSIGNED_CONTEXT ( ( #5743, #6734, #946 ) ) REPRESENTATION_CONTEXT ( 'NONE', 'WORKASPACE' ) );
#7145 = DIRECTION ( 'NONE',  ( -0.000000000000000000, -0.000000000000000000, 1.000000000000000000 ) ) ;
#7146 = CARTESIAN_POINT ( 'NONE',  ( 120.0000000000009948, 45.00000000000008527, 20.00000000000000000 ) ) ;
#7147 = CARTESIAN_POINT ( 'NONE',  ( 31.11163258972580081, 76.09530646335886672, -6.227229208586041231 ) ) ;
#7148 = CARTESIAN_POINT ( 'NONE',  ( 74.16198487095665826, 40.00000000000009237, 25.00000000000000000 ) ) ;
#7149 = PLANE ( 'NONE',  #10234 ) ;
#7150 = CARTESIAN_POINT ( 'NONE',  ( 1.658621287961228566E-16, 111.5624999986344079, 2.708734125000000326 ) ) ;
#7151 = FACE_OUTER_BOUND ( 'NONE', #462, .T. ) ;
#7152 = CARTESIAN_POINT ( 'NONE',  ( 25.00000000000000000, 445.0000000000000568, -29.99999999999998934 ) ) ;
#7153 = ADVANCED_FACE ( 'NONE', ( #2544 ), #862, .T. ) ;
#7154 = EDGE_CURVE ( 'NONE', #11256, #5951, #5662, .T. ) ;
#7155 = EDGE_LOOP ( 'NONE', ( #3105, #1303, #7287, #8340 ) ) ;
#7156 = CARTESIAN_POINT ( 'NONE',  ( 170.0000000000011369, 230.0000000000000853, -19.99999999999999645 ) ) ;
#7157 = ORIENTED_EDGE ( 'NONE', *, *, #5867, .F. ) ;
#7158 = DIRECTION ( 'NONE',  ( 0.000000000000000000, 0.4999999999999990008, -0.8660254037844391517 ) ) ;
#7159 = CARTESIAN_POINT ( 'NONE',  ( 125.0000000000009663, 42.92893218813457423, 25.00000000000000000 ) ) ;
#7160 = VERTEX_POINT ( 'NONE', #8202 ) ;
#7161 = CIRCLE ( 'NONE', #799, 115.0000000000000284 ) ;
#7162 = FACE_OUTER_BOUND ( 'NONE', #126, .T. ) ;
#7163 = DIRECTION ( 'NONE',  ( 1.000000000000000000, -0.000000000000000000, -0.000000000000000000 ) ) ;
#7164 = VERTEX_POINT ( 'NONE', #1613 ) ;
#7165 = CARTESIAN_POINT ( 'NONE',  ( 147.9289321881356045, 20.00000000000009237, 25.00000000000000000 ) ) ;
#7166 = EDGE_CURVE ( 'NONE', #950, #5901, #1266, .T. ) ;
#7167 = ADVANCED_FACE ( 'NONE', ( #9196 ), #674, .T. ) ;
#7168 = AXIS2_PLACEMENT_3D ( 'NONE', #3077, #6065, #6940 ) ;
#7169 = EDGE_LOOP ( 'NONE', ( #682, #7297, #11160, #7754 ) ) ;
#7170 = CARTESIAN_POINT ( 'NONE',  ( 1.990051048614449116E-16, 112.1249999972688158, 3.250000000000000444 ) ) ;
#7171 = FACE_OUTER_BOUND ( 'NONE', #1885, .T. ) ;
#7172 = ORIENTED_EDGE ( 'NONE', *, *, #8884, .T. ) ;
#7173 = DIRECTION ( 'NONE',  ( -0.8660254037844363761, 0.5000000000000038858, 0.000000000000000000 ) ) ;
#7174 = DIRECTION ( 'NONE',  ( 0.000000000000000000, -0.000000000000000000, 1.000000000000000000 ) ) ;
#7175 = ORIENTED_EDGE ( 'NONE', *, *, #5949, .T. ) ;
#7176 = FACE_OUTER_BOUND ( 'NONE', #11925, .T. ) ;
#7178 = CARTESIAN_POINT ( 'NONE',  ( 69.52686081652184669, 40.00000000000009237, -28.12499999999999645 ) ) ;
#7177 = CIRCLE ( 'NONE', #1610, 110.0000000000000284 ) ;
#7179 = FACE_OUTER_BOUND ( 'NONE', #5574, .T. ) ;
#7180 = AXIS2_PLACEMENT_3D ( 'NONE', #8197, #353, #9125 ) ;
#7181 = ORIENTED_EDGE ( 'NONE', *, *, #9998, .F. ) ;
#7182 = ADVANCED_FACE ( 'NONE', ( #6715 ), #11461, .T. ) ;
#7183 = CARTESIAN_POINT ( 'NONE',  ( 3.249999999999999556, 111.9375000000000000, -1.346194077712561166 ) ) ;
#7184 = AXIS2_PLACEMENT_3D ( 'NONE', #11054, #7318, #9290 ) ;
#7185 = CARTESIAN_POINT ( 'NONE',  ( 70.82643617010576520, 18.93883522538484243, 24.89585111362008263 ) ) ;
#7186 = VECTOR ( 'NONE', #8973, 1000.000000000000000 ) ;
#7187 = ORIENTED_EDGE ( 'NONE', *, *, #8703, .T. ) ;
#7188 = CYLINDRICAL_SURFACE ( 'NONE', #11043, 3.250000000000000444 ) ;
#7189 = ORIENTED_EDGE ( 'NONE', *, *, #9406, .T. ) ;
#7190 = DIRECTION ( 'NONE',  ( 0.000000000000000000, 1.000000000000000000, 0.000000000000000000 ) ) ;
#7191 = CARTESIAN_POINT ( 'NONE',  ( 71.69660397288474485, 44.65047563280165122, 22.14258685050887010 ) ) ;
#7192 = VERTEX_POINT ( 'NONE', #2912 ) ;
#7193 = FACE_OUTER_BOUND ( 'NONE', #2929, .T. ) ;
#7194 = EDGE_CURVE ( 'NONE', #12351, #10877, #262, .T. ) ;
#7195 = FACE_OUTER_BOUND ( 'NONE', #142, .T. ) ;
#7196 = DIRECTION ( 'NONE',  ( 0.8660254037844434816, 0.4999999999999913958, 0.000000000000000000 ) ) ;
#7197 = VECTOR ( 'NONE', #5988, 1000.000000000000114 ) ;
#7198 = ORIENTED_EDGE ( 'NONE', *, *, #3119, .T. ) ;
#7199 =( NAMED_UNIT ( * ) SI_UNIT ( $, .STERADIAN. ) SOLID_ANGLE_UNIT ( ) );
#7200 = ORIENTED_EDGE ( 'NONE', *, *, #7194, .T. ) ;
#7201 = AXIS2_PLACEMENT_3D ( 'NONE', #4395, #6397, #8191 ) ;
#7202 = ADVANCED_BREP_SHAPE_REPRESENTATION ( '', ( #589, #1612 ), #9157 ) ;
#7203 = DIRECTION ( 'NONE',  ( -1.000000000000000000, 3.469446951953611033E-15, 0.000000000000000000 ) ) ;
#7204 = CIRCLE ( 'NONE', #631, 9.999999999999994671 ) ;
#7205 = DIRECTION ( 'NONE',  ( 0.000000000000000000, 0.4999999999999962808, -0.8660254037844407060 ) ) ;
#7206 = CARTESIAN_POINT ( 'NONE',  ( 140.0000000000011369, 225.0000000000000853, 25.00000000000000000 ) ) ;
#7207 = LINE ( 'NONE', #9310, #8950 ) ;
#7208 = CARTESIAN_POINT ( 'NONE',  ( 0.000000000000000000, 1.178949249685212974, -2.042000000000001148 ) ) ;
#7209 = CARTESIAN_POINT ( 'NONE',  ( 45.35898384862240107, 85.26794919243110371, 9.660254037844419273 ) ) ;
#7210 = EDGE_CURVE ( 'NONE', #8730, #11587, #985, .T. ) ;
#7211 = DIRECTION ( 'NONE',  ( -0.000000000000000000, 1.000000000000000000, -0.000000000000000000 ) ) ;
#7212 = CARTESIAN_POINT ( 'NONE',  ( 69.72092797052474111, 16.81038406663796536, -27.64057077031494458 ) ) ;
#7213 = CARTESIAN_POINT ( 'NONE',  ( 2.708734125000000326, 114.3124999986344079, 0.000000000000000000 ) ) ;
#7214 = EDGE_CURVE ( 'NONE', #2747, #11089, #1043, .T. ) ;
#7215 = CARTESIAN_POINT ( 'NONE',  ( 2.708734124999999882, 110.5624999986344079, 0.000000000000000000 ) ) ;
#7216 = DIRECTION ( 'NONE',  ( 0.000000000000000000, -0.000000000000000000, 1.000000000000000000 ) ) ;
#7217 = EDGE_CURVE ( 'NONE', #9910, #3039, #7767, .T. ) ;
#7218 = AXIS2_PLACEMENT_3D ( 'NONE', #5836, #6641, #2090 ) ;
#7219 = ORIENTED_EDGE ( 'NONE', *, *, #1282, .F. ) ;
#7220 = PLANE ( 'NONE',  #12216 ) ;
#7221 = ORIENTED_EDGE ( 'NONE', *, *, #6168, .F. ) ;
#7222 = CARTESIAN_POINT ( 'NONE',  ( 25.00000000000000355, 570.2996408614167194, -88.00000000000000000 ) ) ;
#7223 = CARTESIAN_POINT ( 'NONE',  ( 0.000000000000000000, 10.00000000000017586, 0.000000000000000000 ) ) ;
#7224 = VERTEX_POINT ( 'NONE', #9627 ) ;
#7225 = VECTOR ( 'NONE', #7031, 1000.000000000000114 ) ;
#7226 = DIRECTION ( 'NONE',  ( -0.000000000000000000, 0.000000000000000000, 1.000000000000000000 ) ) ;
#7227 = CARTESIAN_POINT ( 'NONE',  ( -31.92482683647865471, 87.00000000000005684, -8.660254037844584474 ) ) ;
#7228 = EDGE_CURVE ( 'NONE', #10685, #6060, #7710, .T. ) ;
#7229 = EDGE_CURVE ( 'NONE', #8, #10079, #4640, .T. ) ;
#7230 = EDGE_LOOP ( 'NONE', ( #6858, #9675, #5295, #547 ) ) ;
#7231 = FACE_OUTER_BOUND ( 'NONE', #5171, .T. ) ;
#7232 = CIRCLE ( 'NONE', #5849, 30.00000000000000355 ) ;
#7233 = VERTEX_POINT ( 'NONE', #6774 ) ;
#7234 = CARTESIAN_POINT ( 'NONE',  ( 29.99337288235791732, 77.98292469156852746, -5.126776908431767588 ) ) ;
#7235 = FACE_OUTER_BOUND ( 'NONE', #2519, .T. ) ;
#7236 = VERTEX_POINT ( 'NONE', #3035 ) ;
#7237 = ORIENTED_EDGE ( 'NONE', *, *, #3045, .T. ) ;
#7238 = DIRECTION ( 'NONE',  ( 0.000000000000000000, 0.000000000000000000, 1.000000000000000000 ) ) ;
#7239 = CARTESIAN_POINT ( 'NONE',  ( 72.02465572632023338, 10.26536114380532894, 20.91766802171319739 ) ) ;
#7240 = ORIENTED_EDGE ( 'NONE', *, *, #5828, .F. ) ;
#7241 = EDGE_CURVE ( 'NONE', #11844, #11089, #6838, .T. ) ;
#7242 = ADVANCED_FACE ( 'NONE', ( #4033 ), #7828, .T. ) ;
#7243 = CARTESIAN_POINT ( 'NONE',  ( 0.000000000000000000, 75.00000000000000000, 0.000000000000000000 ) ) ;
#7244 = DIRECTION ( 'NONE',  ( -1.000000000000000000, 1.387778780781445676E-14, 0.000000000000000000 ) ) ;
#7245 = CARTESIAN_POINT ( 'NONE',  ( 2.500000000000000000, 1.178949249685217415, 2.041999999999998483 ) ) ;
#7246 = CIRCLE ( 'NONE', #12024, 5.000000000000000888 ) ;
#7247 = ORIENTED_EDGE ( 'NONE', *, *, #7083, .T. ) ;
#7248 = DIRECTION ( 'NONE',  ( -0.000000000000000000, -1.000000000000000000, -0.000000000000000000 ) ) ;
#7249 = CARTESIAN_POINT ( 'NONE',  ( 71.06140945339295456, 17.19704224702771356, 24.19089746873543945 ) ) ;
#7250 = EDGE_CURVE ( 'NONE', #1500, #5250, #874, .T. ) ;
#7251 = EDGE_LOOP ( 'NONE', ( #5302, #4126, #2335, #359 ) ) ;
#7252 = DIRECTION ( 'NONE',  ( -0.000000000000000000, -1.000000000000000000, -0.000000000000000000 ) ) ;
#7253 = DIRECTION ( 'NONE',  ( 0.4999999999999977796, -0.8660254037844399289, 0.000000000000000000 ) ) ;
#7254 = CIRCLE ( 'NONE', #4657, 10.00000000000000178 ) ;
#7255 = ORIENTED_EDGE ( 'NONE', *, *, #11133, .T. ) ;
#7256 = AXIS2_PLACEMENT_3D ( 'NONE', #414, #8009, #3286 ) ;
#7257 = FACE_OUTER_BOUND ( 'NONE', #6559, .T. ) ;
#7258 = CARTESIAN_POINT ( 'NONE',  ( 69.62792625627750454, 42.32278466075560175, 27.87393767067159089 ) ) ;
#7259 = ORIENTED_EDGE ( 'NONE', *, *, #10274, .F. ) ;
#7260 = DIRECTION ( 'NONE',  ( -0.000000000000000000, -1.000000000000000000, -0.000000000000000000 ) ) ;
#7261 = CARTESIAN_POINT ( 'NONE',  ( 0.000000000000000000, 265.0000000000000000, 0.000000000000000000 ) ) ;
#7262 = CARTESIAN_POINT ( 'NONE',  ( -1.121994411437819084, 113.6249999986344079, 2.708734125000000326 ) ) ;
#7263 = ORIENTED_EDGE ( 'NONE', *, *, #2183, .F. ) ;
#7264 = VECTOR ( 'NONE', #7989, 1000.000000000000000 ) ;
#7265 = VERTEX_POINT ( 'NONE', #96 ) ;
#7266 = EDGE_CURVE ( 'NONE', #9041, #3006, #7232, .T. ) ;
#7267 = EDGE_CURVE ( 'NONE', #828, #5368, #10450, .T. ) ;
#7268 = PLANE ( 'NONE',  #68 ) ;
#7269 = CARTESIAN_POINT ( 'NONE',  ( 9.942549119892305498, 36.71650635094628967, 80.00000000000000000 ) ) ;
#7271 = EDGE_CURVE ( 'NONE', #6973, #301, #1917, .T. ) ;
#7270 = CARTESIAN_POINT ( 'NONE',  ( 10.02588245322500882, 23.42783121635017451, 80.00000000000000000 ) ) ;
#7272 = VECTOR ( 'NONE', #2485, 1000.000000000000000 ) ;
#7273 = LINE ( 'NONE', #10062, #10381 ) ;
#7274 = VECTOR ( 'NONE', #5191, 1000.000000000000000 ) ;
#7275 = CARTESIAN_POINT ( 'NONE',  ( -27.33018067101281900, 86.99999999999998579, -12.37179148263487782 ) ) ;
#7276 = PLANE ( 'NONE',  #5112 ) ;
#7277 = DIRECTION ( 'NONE',  ( -0.000000000000000000, -1.000000000000000000, -0.000000000000000000 ) ) ;
#7278 = CARTESIAN_POINT ( 'NONE',  ( 2.500000000000000000, -2.357898499370432166, 3.035766082959412415E-15 ) ) ;
#7279 = CARTESIAN_POINT ( 'NONE',  ( 0.000000000000000000, 170.0000000000000000, 0.000000000000000000 ) ) ;
#7280 = DIRECTION ( 'NONE',  ( -0.000000000000000000, 0.8660254037844402619, -0.4999999999999975575 ) ) ;
#7281 = PRESENTATION_LAYER_ASSIGNMENT (  '', '', ( #10655 ) ) ;
#7282 = VECTOR ( 'NONE', #6632, 1000.000000000000000 ) ;
#7283 = CARTESIAN_POINT ( 'NONE',  ( 13.80921887069452758, 30.00000000000009237, 73.71774192269630532 ) ) ;
#7284 = CIRCLE ( 'NONE', #1719, 24.99999999999999645 ) ;
#7285 = ORIENTED_EDGE ( 'NONE', *, *, #6054, .F. ) ;
#7286 = CARTESIAN_POINT ( 'NONE',  ( 1.224646799147353533E-14, 265.0000000000000000, -100.0000000000000284 ) ) ;
#7287 = ORIENTED_EDGE ( 'NONE', *, *, #7299, .F. ) ;
#7288 = DIRECTION ( 'NONE',  ( 0.000000000000000000, 1.000000000000000000, 0.000000000000000000 ) ) ;
#7289 = DIRECTION ( 'NONE',  ( -0.000000000000000000, -1.000000000000000000, -0.000000000000000000 ) ) ;
#7290 = VERTEX_POINT ( 'NONE', #6903 ) ;
#7291 = AXIS2_PLACEMENT_3D ( 'NONE', #10910, #10851, #5188 ) ;
#7292 = DIRECTION ( 'NONE',  ( 0.000000000000000000, 0.000000000000000000, -1.000000000000000000 ) ) ;
#7293 = DIRECTION ( 'NONE',  ( 0.000000000000000000, 0.000000000000000000, 1.000000000000000000 ) ) ;
#7294 = ORIENTED_EDGE ( 'NONE', *, *, #6168, .T. ) ;
#7295 = CARTESIAN_POINT ( 'NONE',  ( 0.000000000000000000, 87.00000000000000000, 24.99999999999999645 ) ) ;
#7296 =( GEOMETRIC_REPRESENTATION_CONTEXT ( 3 ) GLOBAL_UNCERTAINTY_ASSIGNED_CONTEXT ( ( #11003 ) ) GLOBAL_UNIT_ASSIGNED_CONTEXT ( ( #7995, #2459, #5271 ) ) REPRESENTATION_CONTEXT ( 'NONE', 'WORKASPACE' ) );
#7297 = ORIENTED_EDGE ( 'NONE', *, *, #2585, .T. ) ;
#7298 = ORIENTED_EDGE ( 'NONE', *, *, #6551, .F. ) ;
#7299 = EDGE_CURVE ( 'NONE', #3735, #2113, #3456, .T. ) ;
#7300 = DIRECTION ( 'NONE',  ( 0.000000000000000000, 0.000000000000000000, 1.000000000000000000 ) ) ;
#7301 = DIRECTION ( 'NONE',  ( 0.000000000000000000, 0.000000000000000000, 1.000000000000000000 ) ) ;
#7302 = ORIENTED_EDGE ( 'NONE', *, *, #8983, .T. ) ;
#7303 = VECTOR ( 'NONE', #6994, 1000.000000000000000 ) ;
#7304 = FACE_OUTER_BOUND ( 'NONE', #11874, .T. ) ;
#7305 = CARTESIAN_POINT ( 'NONE',  ( -9.976035167149682081, 25.21650635094616533, 79.50000000000000000 ) ) ;
#7306 = ORIENTED_EDGE ( 'NONE', *, *, #153, .T. ) ;
#7307 = CARTESIAN_POINT ( 'NONE',  ( 0.000000000000000000, 0.000000000000000000, 0.000000000000000000 ) ) ;
#7308 = DIRECTION ( 'NONE',  ( 0.000000000000000000, 0.000000000000000000, -1.000000000000000000 ) ) ;
#7309 = CARTESIAN_POINT ( 'NONE',  ( -27.33018067101282256, 87.00000000000000000, -12.37179148263487605 ) ) ;
#7310 = LINE ( 'NONE', #5193, #7186 ) ;
#7311 = ORIENTED_EDGE ( 'NONE', *, *, #7715, .F. ) ;
#7312 = CARTESIAN_POINT ( 'NONE',  ( 1.990051048614449116E-16, 112.2500000000000000, 3.250000000000000444 ) ) ;
#7313 = DIRECTION ( 'NONE',  ( 0.8660254037844377084, -0.5000000000000015543, 0.000000000000000000 ) ) ;
#7314 = AXIS2_PLACEMENT_3D ( 'NONE', #7261, #5456, #6566 ) ;
#7315 = EDGE_CURVE ( 'NONE', #10309, #12150, #5727, .T. ) ;
#7316 = EDGE_CURVE ( 'NONE', #8705, #8944, #10412, .T. ) ;
#7317 = VERTEX_POINT ( 'NONE', #3221 ) ;
#7318 = DIRECTION ( 'NONE',  ( 0.000000000000000000, -0.8660254037844401509, -0.4999999999999974465 ) ) ;
#7319 = CARTESIAN_POINT ( 'NONE',  ( 0.000000000000000000, 110.0000000000000000, 0.000000000000000000 ) ) ;
#7320 = ORIENTED_EDGE ( 'NONE', *, *, #7340, .T. ) ;
#7321 = DIRECTION ( 'NONE',  ( 0.000000000000000000, 0.000000000000000000, -1.000000000000000000 ) ) ;
#7322 = CARTESIAN_POINT ( 'NONE',  ( 76.75496552995652166, 44.83661607564270213, 21.27808286176542296 ) ) ;
#7323 = ORIENTED_EDGE ( 'NONE', *, *, #8878, .T. ) ;
#7324 = CARTESIAN_POINT ( 'NONE',  ( -30.43816488677641985, 80.28464834591375165, 2.971076217724743618 ) ) ;
#7325 = CARTESIAN_POINT ( 'NONE',  ( -27.33018067101282256, 87.00000000000000000, -12.37179148263487605 ) ) ;
#7326 = CARTESIAN_POINT ( 'NONE',  ( 1.915364268218908927, 114.1874999986344079, -1.915364268218909816 ) ) ;
#7327 = CARTESIAN_POINT ( 'NONE',  ( 1.121994411437819084, 113.3749999986344079, -2.708734124999999437 ) ) ;
#7328 = EDGE_CURVE ( 'NONE', #1095, #5931, #10003, .T. ) ;
#7329 = ORIENTED_EDGE ( 'NONE', *, *, #5221, .T. ) ;
#7330 = EDGE_CURVE ( 'NONE', #5470, #4117, #2469, .T. ) ;
#7331 = DIRECTION ( 'NONE',  ( -0.8660254037844398178, -0.4999999999999977796, 0.000000000000000000 ) ) ;
#7332 = DIRECTION ( 'NONE',  ( 0.000000000000000000, 0.000000000000000000, 1.000000000000000000 ) ) ;
#7333 = LINE ( 'NONE', #8376, #7614 ) ;
#7334 = DIRECTION ( 'NONE',  ( 0.000000000000000000, -0.4999999999999976685, -0.8660254037844399289 ) ) ;
#7335 = CARTESIAN_POINT ( 'NONE',  ( -119.9399947101603772, 275.0000000000000000, 35.20508015793608081 ) ) ;
#7336 = CARTESIAN_POINT ( 'NONE',  ( -9.345585736091447160, 42.60014767327400165, 74.41678175564237563 ) ) ;
#7337 = VECTOR ( 'NONE', #2736, 999.9999999999998863 ) ;
#7338 = CARTESIAN_POINT ( 'NONE',  ( 12.41838735530818738, 23.67465209942693960, 73.96505410671836955 ) ) ;
#7339 = CARTESIAN_POINT ( 'NONE',  ( 3.250000000000000444, 111.9374999972688016, 1.346194077712559167 ) ) ;
#7340 = EDGE_CURVE ( 'NONE', #1442, #875, #9207, .T. ) ;
#7341 = CARTESIAN_POINT ( 'NONE',  ( 1.346194077712559389, 112.1875000000000142, 3.250000000000000444 ) ) ;
#7342 = EDGE_CURVE ( 'NONE', #5348, #2246, #5220, .T. ) ;
#7343 = PLANE ( 'NONE',  #2796 ) ;
#7344 = PRODUCT_DEFINITION_FORMATION_WITH_SPECIFIED_SOURCE ( 'ANY', '', #10662, .NOT_KNOWN. ) ;
#7345 = CYLINDRICAL_SURFACE ( 'NONE', #10375, 115.0000000000000284 ) ;
#7346 = ORIENTED_EDGE ( 'NONE', *, *, #9657, .T. ) ;
#7347 = DIRECTION ( 'NONE',  ( 0.9595199576812829534, 0.000000000000000000, -0.2816406412634883671 ) ) ;
#7348 = DIRECTION ( 'NONE',  ( 0.000000000000000000, 0.000000000000000000, 1.000000000000000000 ) ) ;
#7349 = CARTESIAN_POINT ( 'NONE',  ( 74.16198487146469631, 19.66102550257836512, -24.99999999999999645 ) ) ;
#7350 = EDGE_LOOP ( 'NONE', ( #4345, #3127, #1458, #2699 ) ) ;
#7351 = FACE_OUTER_BOUND ( 'NONE', #1679, .T. ) ;
#7352 = EDGE_CURVE ( 'NONE', #8585, #10899, #10815, .T. ) ;
#7353 = LINE ( 'NONE', #12218, #3386 ) ;
#7354 = ORIENTED_EDGE ( 'NONE', *, *, #6298, .F. ) ;
#7355 = LINE ( 'NONE', #2611, #4589 ) ;
#7356 = ORIENTED_EDGE ( 'NONE', *, *, #448, .F. ) ;
#7357 = DIRECTION ( 'NONE',  ( 7.011174048739587977E-15, 1.000000000000000000, 0.000000000000000000 ) ) ;
#7358 = AXIS2_PLACEMENT_3D ( 'NONE', #2018, #5826, #9728 ) ;
#7360 = ORIENTED_EDGE ( 'NONE', *, *, #4773, .T. ) ;
#7359 = DIRECTION ( 'NONE',  ( -0.8660254037844363761, 0.5000000000000038858, 0.000000000000000000 ) ) ;
#7361 = ORIENTED_EDGE ( 'NONE', *, *, #6658, .F. ) ;
#7362 = AXIS2_PLACEMENT_3D ( 'NONE', #4748, #3817, #5000 ) ;
#7363 = PRESENTATION_LAYER_ASSIGNMENT (  '', '', ( #356 ) ) ;
#7364 = CARTESIAN_POINT ( 'NONE',  ( -1.440781129305471087, 43.00000000000008527, 79.50000000000000000 ) ) ;
#7365 = DIRECTION ( 'NONE',  ( 0.000000000000000000, 0.000000000000000000, -1.000000000000000000 ) ) ;
#7366 = EDGE_LOOP ( 'NONE', ( #220, #10233, #6766, #2336, #821 ) ) ;
#7367 = SURFACE_SIDE_STYLE ('',( #1692 ) ) ;
#7368 = DIRECTION ( 'NONE',  ( -1.000000000000000000, 0.000000000000000000, -0.000000000000000000 ) ) ;
#7369 = CARTESIAN_POINT ( 'NONE',  ( 0.000000000000000000, 122.0000000000000000, -22.00000000000000355 ) ) ;
#7370 = CARTESIAN_POINT ( 'NONE',  ( 0.000000000000000000, 122.5000000000000000, 0.000000000000000000 ) ) ;
#7371 = ORIENTED_EDGE ( 'NONE', *, *, #5168, .F. ) ;
#7372 = CARTESIAN_POINT ( 'NONE',  ( -1.121994411437820194, 113.2499999986344079, -2.708734124999999437 ) ) ;
#7373 = ADVANCED_FACE ( 'NONE', ( #4151 ), #7885, .T. ) ;
#7374 = CYLINDRICAL_SURFACE ( 'NONE', #2189, 5.000000000000004441 ) ;
#7375 = AXIS2_PLACEMENT_3D ( 'NONE', #2856, #6542, #10330 ) ;
#7376 = EDGE_CURVE ( 'NONE', #10768, #6205, #3345, .T. ) ;
#7377 = ORIENTED_EDGE ( 'NONE', *, *, #1845, .T. ) ;
#7378 = CARTESIAN_POINT ( 'NONE',  ( 0.000000000000000000, 0.000000000000000000, 79.50000000000000000 ) ) ;
#7379 = LINE ( 'NONE', #2878, #8840 ) ;
#7380 = ORIENTED_EDGE ( 'NONE', *, *, #7644, .F. ) ;
#7381 = CARTESIAN_POINT ( 'NONE',  ( 5.092712519748452848, 41.38333024919784719, 79.50000000000000000 ) ) ;
#7382 = DIRECTION ( 'NONE',  ( -0.000000000000000000, -1.000000000000000000, -0.000000000000000000 ) ) ;
#7383 = EDGE_LOOP ( 'NONE', ( #9289, #11216, #11732, #518 ) ) ;
#7384 = PLANE ( 'NONE',  #9795 ) ;
#7385 = CIRCLE ( 'NONE', #7180, 5.000000000000000888 ) ;
#7386 = CIRCLE ( 'NONE', #9760, 17.00000000000000000 ) ;
#7387 = CARTESIAN_POINT ( 'NONE',  ( 0.000000000000000000, 92.00000000000000000, -22.00000000000000355 ) ) ;
#7388 = CYLINDRICAL_SURFACE ( 'NONE', #9963, 5.000000000000004441 ) ;
#7389 = CARTESIAN_POINT ( 'NONE',  ( 1.915364268218909150, 112.6874999986344079, 1.915364268218909150 ) ) ;
#7390 = ADVANCED_FACE ( 'NONE', ( #9937 ), #5050, .F. ) ;
#7391 = ORIENTED_EDGE ( 'NONE', *, *, #4978, .T. ) ;
#7392 = CIRCLE ( 'NONE', #6584, 70.00000000000001421 ) ;
#7393 = EDGE_CURVE ( 'NONE', #5602, #872, #7030, .T. ) ;
#7394 = DIRECTION ( 'NONE',  ( 7.011174048739587977E-15, 1.000000000000000000, 0.000000000000000000 ) ) ;
#7395 = CARTESIAN_POINT ( 'NONE',  ( -9.976035167149682081, 25.21650635094616533, 79.50000000000000000 ) ) ;
#7396 = AXIS2_PLACEMENT_3D ( 'NONE', #1976, #5786, #4915 ) ;
#7397 = DIRECTION ( 'NONE',  ( 1.000000000000000000, -0.000000000000000000, 0.000000000000000000 ) ) ;
#7398 = CYLINDRICAL_SURFACE ( 'NONE', #8385, 125.0000000000000284 ) ;
#7399 = CARTESIAN_POINT ( 'NONE',  ( -8.500000000000000000, 122.5000000000000000, -6.164414002968973350 ) ) ;
#7400 = AXIS2_PLACEMENT_3D ( 'NONE', #2061, #5866, #4805 ) ;
#7401 = CARTESIAN_POINT ( 'NONE',  ( -15.31738143124597151, 35.07030106808286263, 73.41937046907847275 ) ) ;
#7402 = CARTESIAN_POINT ( 'NONE',  ( 1.990051048614449116E-16, 114.1249999972688158, 3.250000000000000444 ) ) ;
#7403 = EDGE_CURVE ( 'NONE', #9072, #8789, #8129, .T. ) ;
#7404 = EDGE_CURVE ( 'NONE', #3822, #5087, #1860, .T. ) ;
#7405 = CARTESIAN_POINT ( 'NONE',  ( 2.298097038856279806, 111.1250000000000000, 2.298097038856279806 ) ) ;
#7406 = DIRECTION ( 'NONE',  ( 3.469446951953611033E-15, 1.000000000000000000, 0.000000000000000000 ) ) ;
#7407 = AXIS2_PLACEMENT_3D ( 'NONE', #2533, #2590, #1724 ) ;
#7408 = VECTOR ( 'NONE', #10407, 1000.000000000000000 ) ;
#7409 = CARTESIAN_POINT ( 'NONE',  ( 1.088204915335219061E-15, 15.04734002586538821, 75.00000000000001421 ) ) ;
#7410 = VERTEX_POINT ( 'NONE', #5279 ) ;
#7411 = CARTESIAN_POINT ( 'NONE',  ( 0.000000000000000000, 87.50000000000000000, -17.50000000000000000 ) ) ;
#7412 = CARTESIAN_POINT ( 'NONE',  ( -8.500000000000000000, 165.5000000000000000, -6.164414002968973350 ) ) ;
#7413 = CARTESIAN_POINT ( 'NONE',  ( 70.86094439463602157, 18.52957660828512587, -24.79386831724005091 ) ) ;
#7414 = EDGE_LOOP ( 'NONE', ( #5065, #4377, #11162, #5713, #245, #7346, #7639, #3918, #1267, #8752, #8914, #1764 ) ) ;
#7415 =( REPRESENTATION_RELATIONSHIP ('NONE','NONE', #3713, #9674 ) REPRESENTATION_RELATIONSHIP_WITH_TRANSFORMATION ( #11833 )SHAPE_REPRESENTATION_RELATIONSHIP( ) );
#7416 = DIRECTION ( 'NONE',  ( 0.000000000000000000, 1.000000000000000000, 0.000000000000000000 ) ) ;
#7417 = PLANE ( 'NONE',  #11742 ) ;
#7418 = ORIENTED_EDGE ( 'NONE', *, *, #435, .T. ) ;
#7419 = DIRECTION ( 'NONE',  ( -1.000000000000000000, 1.387778780781445676E-14, 0.000000000000000000 ) ) ;
#7420 = ORIENTED_EDGE ( 'NONE', *, *, #10536, .T. ) ;
#7421 = EDGE_CURVE ( 'NONE', #5427, #11988, #468, .T. ) ;
#7422 = AXIS2_PLACEMENT_3D ( 'NONE', #273, #11695, #5956 ) ;
#7423 = DIRECTION ( 'NONE',  ( -0.000000000000000000, -1.000000000000000000, -0.000000000000000000 ) ) ;
#7425 = ORIENTED_EDGE ( 'NONE', *, *, #1152, .F. ) ;
#7424 = CARTESIAN_POINT ( 'NONE',  ( 25.00000000000000000, 345.0000000000000568, -90.00000000000000000 ) ) ;
#7426 = ORIENTED_EDGE ( 'NONE', *, *, #5135, .T. ) ;
#7427 = FACE_OUTER_BOUND ( 'NONE', #8280, .T. ) ;
#7428 = CARTESIAN_POINT ( 'NONE',  ( -29.99337288235791732, 77.98292469156852746, 5.126776908431767588 ) ) ;
#7429 = ORIENTED_EDGE ( 'NONE', *, *, #701, .T. ) ;
#7430 = EDGE_CURVE ( 'NONE', #7410, #11037, #10421, .T. ) ;
#7431 = CARTESIAN_POINT ( 'NONE',  ( 0.000000000000000000, 265.0000000000000000, 0.000000000000000000 ) ) ;
#7432 = PLANE ( 'NONE',  #2621 ) ;
#7433 = PLANE ( 'NONE',  #2808 ) ;
#7434 = EDGE_LOOP ( 'NONE', ( #6549, #2230, #6684, #8774 ) ) ;
#7435 = CARTESIAN_POINT ( 'NONE',  ( 1.915364268218908705, 112.4374999986344079, -1.915364268218909594 ) ) ;
#7436 = VECTOR ( 'NONE', #6972, 1000.000000000000000 ) ;
#7437 = CARTESIAN_POINT ( 'NONE',  ( 3.249999999999999556, 113.9375000000000000, -1.346194077712561166 ) ) ;
#7438 = ORIENTED_EDGE ( 'NONE', *, *, #2965, .F. ) ;
#7439 = CARTESIAN_POINT ( 'NONE',  ( 97.61745645431939522, 275.0000000000000000, 78.07581056504676553 ) ) ;
#7440 = CARTESIAN_POINT ( 'NONE',  ( -16.16361926974168384, 28.95936500225007748, 73.23756171298010997 ) ) ;
#7441 = ORIENTED_EDGE ( 'NONE', *, *, #4266, .T. ) ;
#7442 = DIRECTION ( 'NONE',  ( -0.8660254037844403729, -0.4999999999999970024, 0.000000000000000000 ) ) ;
#7443 = CARTESIAN_POINT ( 'NONE',  ( 72.28042146286416880, 45.16208194665043862, 20.04664579644909139 ) ) ;
#7444 = VECTOR ( 'NONE', #2281, 1000.000000000000000 ) ;
#7445 = VERTEX_POINT ( 'NONE', #407 ) ;
#7446 = CARTESIAN_POINT ( 'NONE',  ( -6.407287480251453893, 38.53525403784446723, 80.00000000000000000 ) ) ;
#7447 = PLANE ( 'NONE',  #2012 ) ;
#7448 = CARTESIAN_POINT ( 'NONE',  ( 2.708734124999999437, 112.4999999986344079, -1.121994411437820638 ) ) ;
#7449 = CARTESIAN_POINT ( 'NONE',  ( 2.708734124999999437, 111.4999999986343937, -1.121994411437820416 ) ) ;
#7450 = VERTEX_POINT ( 'NONE', #8004 ) ;
#7451 = EDGE_LOOP ( 'NONE', ( #6490, #8355, #3689, #6404 ) ) ;
#7452 = VECTOR ( 'NONE', #6947, 1000.000000000000000 ) ;
#7453 = AXIS2_PLACEMENT_3D ( 'NONE', #11025, #9896, #10021 ) ;
#7454 = CARTESIAN_POINT ( 'NONE',  ( -14.18837706086142525, 29.75000000000008882, 80.00000000000000000 ) ) ;
#7455 = CARTESIAN_POINT ( 'NONE',  ( 3.061616997868383043E-15, 65.00000000000000000, -25.00000000000000000 ) ) ;
#7456 = EDGE_CURVE ( 'NONE', #7513, #5974, #7246, .T. ) ;
#7457 = CARTESIAN_POINT ( 'NONE',  ( -33.37417589188917333, 76.99999999999998579, 8.451338748825380165 ) ) ;
#7458 = DIRECTION ( 'NONE',  ( 0.000000000000000000, 0.000000000000000000, 1.000000000000000000 ) ) ;
#7459 = CARTESIAN_POINT ( 'NONE',  ( -14.19078112930533031, 30.08333333333487403, 80.00000000000000000 ) ) ;
#7460 = DIRECTION ( 'NONE',  ( 0.000000000000000000, 1.000000000000000000, 0.000000000000000000 ) ) ;
#7461 = PLANE ( 'NONE',  #2828 ) ;
#7462 = CIRCLE ( 'NONE', #2671, 25.00000000000000000 ) ;
#7463 = VECTOR ( 'NONE', #4040, 1000.000000000000000 ) ;
#7464 = DIRECTION ( 'NONE',  ( -0.000000000000000000, -1.000000000000000000, -0.000000000000000000 ) ) ;
#7465 = EDGE_CURVE ( 'NONE', #6241, #7101, #9746, .T. ) ;
#7466 = EDGE_CURVE ( 'NONE', #421, #5123, #6271, .T. ) ;
#7467 = AXIS2_PLACEMENT_3D ( 'NONE', #299, #11717, #6044 ) ;
#7468 = CARTESIAN_POINT ( 'NONE',  ( 6.215335591258955183, 16.92236976696375805, 74.74677668485156801 ) ) ;
#7469 = VECTOR ( 'NONE', #7854, 1000.000000000000000 ) ;
#7470 = CARTESIAN_POINT ( 'NONE',  ( -12.57411137850303540, 36.28349364905398033, 80.00000000000000000 ) ) ;
#7471 = ORIENTED_EDGE ( 'NONE', *, *, #8287, .T. ) ;
#7472 = CARTESIAN_POINT ( 'NONE',  ( -25.00000000000000000, 450.0000000000000568, -59.99999999999999289 ) ) ;
#7473 = CARTESIAN_POINT ( 'NONE',  ( 0.000000000000000000, 0.000000000000000000, 79.50000000000000000 ) ) ;
#7474 = VERTEX_POINT ( 'NONE', #11704 ) ;
#7475 = CARTESIAN_POINT ( 'NONE',  ( 0.000000000000000000, 75.00000000000001421, -17.00000000000000000 ) ) ;
#7476 = FACE_OUTER_BOUND ( 'NONE', #3162, .T. ) ;
#7477 = AXIS2_PLACEMENT_3D ( 'NONE', #9026, #7112, #7301 ) ;
#7478 = ORIENTED_EDGE ( 'NONE', *, *, #8506, .F. ) ;
#7479 = CARTESIAN_POINT ( 'NONE',  ( -20.00000000000000355, 50.00000000000000000, 57.08203932499370836 ) ) ;
#7480 = EDGE_CURVE ( 'NONE', #1112, #7967, #11018, .T. ) ;
#7481 = ORIENTED_EDGE ( 'NONE', *, *, #8924, .T. ) ;
#7482 = DIRECTION ( 'NONE',  ( 0.000000000000000000, 1.000000000000000000, 0.000000000000000000 ) ) ;
#7483 = DIRECTION ( 'NONE',  ( -1.000000000000000000, 0.000000000000000000, 0.000000000000000000 ) ) ;
#7484 = VERTEX_POINT ( 'NONE', #9814 ) ;
#7485 = CIRCLE ( 'NONE', #7291, 75.00000000000001421 ) ;
#7486 = EDGE_LOOP ( 'NONE', ( #1, #2942, #12266, #9135, #4306 ) ) ;
#7487 = FILL_AREA_STYLE ('',( #822 ) ) ;
#7488 = CARTESIAN_POINT ( 'NONE',  ( 10.19254911989230727, 36.28349364905406560, 79.50000000000000000 ) ) ;
#7489 = VECTOR ( 'NONE', #7289, 1000.000000000000000 ) ;
#7490 = CARTESIAN_POINT ( 'NONE',  ( 89.80805993797383735, 275.0000000000000000, 71.82974571984303225 ) ) ;
#7491 = CARTESIAN_POINT ( 'NONE',  ( 82.90657655638969459, 275.0000000000000000, 79.06642500897268633 ) ) ;
#7492 = VERTEX_POINT ( 'NONE', #8881 ) ;
#7493 = CARTESIAN_POINT ( 'NONE',  ( 1.915364268218909594, 110.4374999986344079, 1.915364268218909594 ) ) ;
#7494 = EDGE_CURVE ( 'NONE', #6826, #12189, #267, .T. ) ;
#7495 = EDGE_CURVE ( 'NONE', #11350, #3728, #3236, .T. ) ;
#7496 = CARTESIAN_POINT ( 'NONE',  ( -0.9407811293054709756, 40.00000000000008527, 79.50000000000000000 ) ) ;
#7497 = MECHANICAL_DESIGN_GEOMETRIC_PRESENTATION_REPRESENTATION (  '', ( #11886 ), #7296 ) ;
#7498 = ORIENTED_EDGE ( 'NONE', *, *, #4563, .F. ) ;
#7499 = FACE_OUTER_BOUND ( 'NONE', #8623, .T. ) ;
#7500 = CARTESIAN_POINT ( 'NONE',  ( 70.63701798748766691, 47.25584164860985226, 25.20839359252511969 ) ) ;
#7501 = ORIENTED_EDGE ( 'NONE', *, *, #8805, .T. ) ;
#7502 = CARTESIAN_POINT ( 'NONE',  ( 3.250000000000000444, 110.0000000000000000, 0.000000000000000000 ) ) ;
#7503 = CARTESIAN_POINT ( 'NONE',  ( 0.000000000000000000, 50.00000000000000000, 0.000000000000000000 ) ) ;
#7504 = ORIENTED_EDGE ( 'NONE', *, *, #3269, .F. ) ;
#7505 = DIRECTION ( 'NONE',  ( 0.000000000000000000, -1.287488025362403787E-15, -1.000000000000000000 ) ) ;
#7506 = CARTESIAN_POINT ( 'NONE',  ( 0.000000000000000000, 345.0000000000000568, 0.000000000000000000 ) ) ;
#7507 = CARTESIAN_POINT ( 'NONE',  ( -2.708734125000000326, 111.1249999986343937, -1.121994411437818195 ) ) ;
#7508 = VECTOR ( 'NONE', #6628, 1000.000000000000000 ) ;
#7509 = ORIENTED_EDGE ( 'NONE', *, *, #3844, .T. ) ;
#7510 = ORIENTED_EDGE ( 'NONE', *, *, #1657, .T. ) ;
#7511 = DIRECTION ( 'NONE',  ( 0.7071067811865513475, 0.7071067811865437980, 0.000000000000000000 ) ) ;
#7512 = DIRECTION ( 'NONE',  ( -1.000000000000000000, -0.000000000000000000, -0.000000000000000000 ) ) ;
#7513 = VERTEX_POINT ( 'NONE', #8254 ) ;
#7514 = CARTESIAN_POINT ( 'NONE',  ( 4.025725221640669815, 38.53525403784453118, 80.00000000000000000 ) ) ;
#7515 = CARTESIAN_POINT ( 'NONE',  ( 0.000000000000000000, 50.00000000000000000, 0.000000000000000000 ) ) ;
#7516 =( BOUNDED_CURVE ( )  B_SPLINE_CURVE ( 3, ( #3346, #7944, #3279, #11771 ),
 .UNSPECIFIED., .F., .F. ) 
 B_SPLINE_CURVE_WITH_KNOTS ( ( 4, 4 ),
 ( 1.860548028230944562, 2.013707370868536461 ),
 .UNSPECIFIED. ) 
 CURVE ( )  GEOMETRIC_REPRESENTATION_ITEM ( )  RATIONAL_B_SPLINE_CURVE ( ( 1.000000000000000000, 0.9980461397859388128, 0.9980461397859388128, 1.000000000000000000 ) ) 
 REPRESENTATION_ITEM ( '' )  );
#7517 = CARTESIAN_POINT ( 'NONE',  ( -6.407287480251391720, 21.46474596215567487, 79.50000000000000000 ) ) ;
#7518 = CARTESIAN_POINT ( 'NONE',  ( 0.000000000000000000, 52.00000000000000711, -73.00000000000002842 ) ) ;
#7519 = LINE ( 'NONE', #5595, #5194 ) ;
#7520 = EDGE_CURVE ( 'NONE', #4819, #5619, #654, .T. ) ;
#7521 = EDGE_CURVE ( 'NONE', #3440, #1199, #11074, .T. ) ;
#7522 = UNCERTAINTY_MEASURE_WITH_UNIT (LENGTH_MEASURE( 1.000000000000000082E-05 ), #5830, 'distance_accuracy_value', 'NONE');
#7523 = DIRECTION ( 'NONE',  ( 0.000000000000000000, 0.7071067811865514585, 0.7071067811865435759 ) ) ;
#7524 = LINE ( 'NONE', #6588, #8263 ) ;
#7525 = VERTEX_POINT ( 'NONE', #4457 ) ;
#7526 = CIRCLE ( 'NONE', #5541, 17.50000000000000000 ) ;
#7527 = DIRECTION ( 'NONE',  ( 0.000000000000000000, 0.000000000000000000, -1.000000000000000000 ) ) ;
#7528 = DIRECTION ( 'NONE',  ( -0.000000000000000000, -1.000000000000000000, -0.000000000000000000 ) ) ;
#7529 = CARTESIAN_POINT ( 'NONE',  ( 74.26978800665389713, 18.83860766962025224, -24.86610009102977159 ) ) ;
#7530 = EDGE_LOOP ( 'NONE', ( #2584, #6420, #10560, #5526 ) ) ;
#7531 = CARTESIAN_POINT ( 'NONE',  ( 2.694222958124177204E-15, 127.0000000000000000, 22.00000000000000355 ) ) ;
#7532 = CARTESIAN_POINT ( 'NONE',  ( 0.000000000000000000, 77.00000000000000000, -30.00000000000000000 ) ) ;
#7533 = ORIENTED_EDGE ( 'NONE', *, *, #5111, .F. ) ;
#7534 = DIRECTION ( 'NONE',  ( -0.8660254037844403729, -0.4999999999999970579, 0.000000000000000000 ) ) ;
#7535 = VECTOR ( 'NONE', #20, 1000.000000000000114 ) ;
#7536 = EDGE_CURVE ( 'NONE', #2084, #11256, #4525, .T. ) ;
#7537 = CARTESIAN_POINT ( 'NONE',  ( 3.250000000000000444, 110.8749999972688158, 0.000000000000000000 ) ) ;
#7538 =( BOUNDED_SURFACE ( )  B_SPLINE_SURFACE ( 3, 2, ( 
 ( #4584, #10251, #7275 ),
 ( #2534, #1600, #5532 ),
 ( #10064, #9311, #9121 ),
 ( #11201, #3652, #6335 ) ),
 .UNSPECIFIED., .F., .F., .F. ) 
 B_SPLINE_SURFACE_WITH_KNOTS ( ( 4, 4 ),
 ( 3, 3 ),
 ( 5.137468306293111020, 5.139829129961272614 ),
 ( 0.7666061298070812047, 1.000000000000000000 ),
 .UNSPECIFIED. ) 
 GEOMETRIC_REPRESENTATION_ITEM ( )  RATIONAL_B_SPLINE_SURFACE ( (
 ( 0.9369318869591372057, 0.9588653738936746551, 1.000000000000000000),
 ( 0.9369993130727753972, 0.9589093509185225850, 1.000000000000000000),
 ( 0.9370666800230464943, 0.9589532893555189341, 1.000000000000000000),
 ( 0.9371339877439295307, 0.9589971891616031474, 1.000000000000000000) ) ) 
 REPRESENTATION_ITEM ( '' )  SURFACE ( )  );
#7539 = ORIENTED_EDGE ( 'NONE', *, *, #2181, .T. ) ;
#7540 = CARTESIAN_POINT ( 'NONE',  ( 5.092712519748611832, 18.61666975080242992, 80.00000000000000000 ) ) ;
#7541 = DIRECTION ( 'NONE',  ( -5.551115123125782702E-15, -0.4999999999999976685, 0.8660254037844399289 ) ) ;
#7542 = ORIENTED_EDGE ( 'NONE', *, *, #10146, .T. ) ;
#7543 = CARTESIAN_POINT ( 'NONE',  ( -1.346194077712555837, 111.5624999972688158, -3.250000000000004885 ) ) ;
#7544 = EDGE_LOOP ( 'NONE', ( #8817, #971 ) ) ;
#7545 = DIRECTION ( 'NONE',  ( -0.5000000000000006661, -0.8660254037844383745, 0.000000000000000000 ) ) ;
#7546 = CARTESIAN_POINT ( 'NONE',  ( 11.80681480225048396, 30.25000000000018474, 80.00000000000000000 ) ) ;
#7547 = DIRECTION ( 'NONE',  ( 1.387778780781445676E-14, 1.000000000000000000, 0.000000000000000000 ) ) ;
#7548 = EDGE_CURVE ( 'NONE', #9474, #9178, #3531, .T. ) ;
#7549 = EDGE_CURVE ( 'NONE', #9708, #11877, #7333, .T. ) ;
#7550 = VERTEX_POINT ( 'NONE', #7514 ) ;
#7551 = CARTESIAN_POINT ( 'NONE',  ( 1.915364268218909150, 113.6874999986344079, 1.915364268218909150 ) ) ;
#7552 = PLANE ( 'NONE',  #5006 ) ;
#7553 = VECTOR ( 'NONE', #8764, 1000.000000000000000 ) ;
#7554 = VECTOR ( 'NONE', #10665, 1000.000000000000000 ) ;
#7555 = ORIENTED_EDGE ( 'NONE', *, *, #2351, .T. ) ;
#7556 = FACE_OUTER_BOUND ( 'NONE', #8051, .T. ) ;
#7557 = PLANE ( 'NONE',  #10443 ) ;
#7558 = VERTEX_POINT ( 'NONE', #661 ) ;
#7559 = CARTESIAN_POINT ( 'NONE',  ( 5.092712519748452848, 41.38333024919784719, 80.00000000000000000 ) ) ;
#7560 = CARTESIAN_POINT ( 'NONE',  ( 0.000000000000000000, 216.0365690573663926, 0.000000000000000000 ) ) ;
#7561 = ORIENTED_EDGE ( 'NONE', *, *, #2351, .F. ) ;
#7562 = DIRECTION ( 'NONE',  ( 0.000000000000000000, 0.000000000000000000, 1.000000000000000000 ) ) ;
#7563 = DIRECTION ( 'NONE',  ( -0.4999999999999978351, 0.000000000000000000, 0.8660254037844399289 ) ) ;
#7564 = VECTOR ( 'NONE', #622, 1000.000000000000000 ) ;
#7565 = DIRECTION ( 'NONE',  ( -1.000000000000000000, 0.000000000000000000, -0.000000000000000000 ) ) ;
#7566 = TOROIDAL_SURFACE ( 'NONE', #10751, 10.00000000000000000, 5.000000000000000000 ) ;
#7567 = CARTESIAN_POINT ( 'NONE',  ( 0.000000000000000000, 63.00000000000000000, -57.08203932499371547 ) ) ;
#7568 = EDGE_LOOP ( 'NONE', ( #3618, #3832, #12304, #7594, #2299, #628, #4619, #2731, #4165, #7198 ) ) ;
#7569 = ORIENTED_EDGE ( 'NONE', *, *, #10326, .T. ) ;
#7570 = AXIS2_PLACEMENT_3D ( 'NONE', #4223, #5349, #4285 ) ;
#7571 = CARTESIAN_POINT ( 'NONE',  ( -20.00000000000000355, 7.965803112215716020, -57.08203932499370836 ) ) ;
#7572 = EDGE_CURVE ( 'NONE', #1420, #11972, #4337, .T. ) ;
#7573 = CARTESIAN_POINT ( 'NONE',  ( 0.000000000000000000, 165.5000000000000000, -10.49999999999999822 ) ) ;
#7574 = ORIENTED_EDGE ( 'NONE', *, *, #8369, .T. ) ;
#7575 = CARTESIAN_POINT ( 'NONE',  ( 0.000000000000000000, 52.00000000000000711, 0.000000000000000000 ) ) ;
#7576 = LINE ( 'NONE', #1035, #6557 ) ;
#7577 = LINE ( 'NONE', #5656, #4415 ) ;
#7578 = VERTEX_POINT ( 'NONE', #3649 ) ;
#7579 = AXIS2_PLACEMENT_3D ( 'NONE', #4949, #3950, #8794 ) ;
#7580 = COLOUR_RGB ( '', 0.40784314, 0.44705882, 0.49803922) ;
#7581 = CARTESIAN_POINT ( 'NONE',  ( 74.16198487095664404, 40.00000000000008527, -25.00000000000000000 ) ) ;
#7582 = FACE_OUTER_BOUND ( 'NONE', #10521, .T. ) ;
#7583 = ORIENTED_EDGE ( 'NONE', *, *, #11393, .F. ) ;
#7584 = CIRCLE ( 'NONE', #2213, 115.0000000000000284 ) ;
#7585 = EDGE_CURVE ( 'NONE', #737, #8283, #8598, .T. ) ;
#7586 = CARTESIAN_POINT ( 'NONE',  ( -12.32411137850302119, 23.28349364905396612, 79.50000000000000000 ) ) ;
#7587 = CARTESIAN_POINT ( 'NONE',  ( 8.266365894244636700E-15, -10.00000000000000000, 65.00000000000001421 ) ) ;
#7588 = CARTESIAN_POINT ( 'NONE',  ( 69.77609205918946600, 16.39783078570843244, -27.50116345873387758 ) ) ;
#7589 = VERTEX_POINT ( 'NONE', #2712 ) ;
#7590 = CARTESIAN_POINT ( 'NONE',  ( 2.500000000000000000, 1.178949249685212974, -2.042000000000001148 ) ) ;
#7591 = ADVANCED_FACE ( 'NONE', ( #11198 ), #3468, .T. ) ;
#7592 = FACE_OUTER_BOUND ( 'NONE', #4625, .T. ) ;
#7593 = AXIS2_PLACEMENT_3D ( 'NONE', #3313, #3442, #3497 ) ;
#7594 = ORIENTED_EDGE ( 'NONE', *, *, #7549, .T. ) ;
#7595 = CARTESIAN_POINT ( 'NONE',  ( 2.979367062500000163, 110.7187499979516190, 0.000000000000000000 ) ) ;
#7596 = AXIS2_PLACEMENT_3D ( 'NONE', #6553, #2742, #1939 ) ;
#7597 = EDGE_CURVE ( 'NONE', #12062, #12288, #5979, .T. ) ;
#7598 = ORIENTED_EDGE ( 'NONE', *, *, #9659, .T. ) ;
#7599 = CARTESIAN_POINT ( 'NONE',  ( 2.708734124999999882, 114.4374999986344079, 0.000000000000000000 ) ) ;
#7600 = DIRECTION ( 'NONE',  ( -0.000000000000000000, -1.000000000000000000, -0.000000000000000000 ) ) ;
#7601 = ORIENTED_EDGE ( 'NONE', *, *, #9614, .F. ) ;
#7602 = CARTESIAN_POINT ( 'NONE',  ( 31.52024609858349180, 77.00000000000001421, -7.288261850756687643 ) ) ;
#7603 = FACE_OUTER_BOUND ( 'NONE', #10890, .T. ) ;
#7604 = ORIENTED_EDGE ( 'NONE', *, *, #9673, .T. ) ;
#7605 = EDGE_CURVE ( 'NONE', #11491, #10191, #12261, .T. ) ;
#7606 = EDGE_CURVE ( 'NONE', #10138, #11537, #5404, .T. ) ;
#7607 = CARTESIAN_POINT ( 'NONE',  ( 165.0000000000011369, 225.0000000000000853, 25.00000000000000000 ) ) ;
#7608 = PLANE ( 'NONE',  #7596 ) ;
#7609 = DIRECTION ( 'NONE',  ( -0.8660254037844365982, 0.5000000000000036637, 0.000000000000000000 ) ) ;
#7610 =( BOUNDED_CURVE ( )  B_SPLINE_CURVE ( 3, ( #3134, #9851, #1448, #506 ),
 .UNSPECIFIED., .F., .F. ) 
 B_SPLINE_CURVE_WITH_KNOTS ( ( 4, 4 ),
 ( 4.284962911267360397, 4.868362425771961099 ),
 .UNSPECIFIED. ) 
 CURVE ( )  GEOMETRIC_REPRESENTATION_ITEM ( )  RATIONAL_B_SPLINE_CURVE ( ( 1.000000000000000000, 0.9718376280744367435, 0.9718376280744367435, 1.000000000000000000 ) ) 
 REPRESENTATION_ITEM ( '' )  );
#7611 = ORIENTED_EDGE ( 'NONE', *, *, #7494, .T. ) ;
#7612 = CARTESIAN_POINT ( 'NONE',  ( -2.708734125000000326, 111.1249999986343937, -1.121994411437818195 ) ) ;
#7613 = CARTESIAN_POINT ( 'NONE',  ( -2.298097038856279362, 113.2499999972688158, 2.298097038856279806 ) ) ;
#7614 = VECTOR ( 'NONE', #7397, 1000.000000000000000 ) ;
#7615 = ORIENTED_EDGE ( 'NONE', *, *, #5382, .T. ) ;
#7616 = DIRECTION ( 'NONE',  ( 0.000000000000000000, 0.000000000000000000, 1.000000000000000000 ) ) ;
#7617 = EDGE_CURVE ( 'NONE', #80, #5761, #8190, .T. ) ;
#7618 = CARTESIAN_POINT ( 'NONE',  ( 70.00771527461461119, 44.96961139197239277, 26.90815449096327683 ) ) ;
#7619 = ORIENTED_EDGE ( 'NONE', *, *, #2249, .F. ) ;
#7620 = CARTESIAN_POINT ( 'NONE',  ( 0.000000000000000000, 77.00000000000000000, 0.000000000000000000 ) ) ;
#7621 = CARTESIAN_POINT ( 'NONE',  ( 69.53296405455486706, 19.34582284458782553, 28.10992626845828113 ) ) ;
#7622 = EDGE_LOOP ( 'NONE', ( #11192, #9797 ) ) ;
#7623 = DIRECTION ( 'NONE',  ( 0.000000000000000000, -0.4999999999999965028, 0.8660254037844407060 ) ) ;
#7624 = CARTESIAN_POINT ( 'NONE',  ( 135.0000000000011084, 67.07106781186550393, 25.00000000000000000 ) ) ;
#7625 = AXIS2_PLACEMENT_3D ( 'NONE', #4729, #6606, #10400 ) ;
#7626 = CARTESIAN_POINT ( 'NONE',  ( 0.000000000000000000, 265.0000000000000000, -17.00000000000000000 ) ) ;
#7627 = FACE_OUTER_BOUND ( 'NONE', #4017, .T. ) ;
#7628 = CARTESIAN_POINT ( 'NONE',  ( 1.121994411437819084, 111.7499999986343795, 2.708734124999999882 ) ) ;
#7629 = VERTEX_POINT ( 'NONE', #23 ) ;
#7630 = SURFACE_STYLE_FILL_AREA ( #8490 ) ;
#7631 = ORIENTED_EDGE ( 'NONE', *, *, #8275, .F. ) ;
#7632 = DIRECTION ( 'NONE',  ( 0.000000000000000000, 0.000000000000000000, 1.000000000000000000 ) ) ;
#7633 = CARTESIAN_POINT ( 'NONE',  ( 9.182979779718706936, 40.84457429296963227, 74.43652437870400718 ) ) ;
#7634 = VERTEX_POINT ( 'NONE', #4765 ) ;
#7635 = CARTESIAN_POINT ( 'NONE',  ( 0.000000000000000000, 65.00000000000000000, 0.000000000000000000 ) ) ;
#7636 = DIRECTION ( 'NONE',  ( 1.000000000000000000, 0.000000000000000000, 0.000000000000000000 ) ) ;
#7637 = DIRECTION ( 'NONE',  ( 0.000000000000000000, 1.000000000000000000, 0.000000000000000000 ) ) ;
#7638 = FACE_OUTER_BOUND ( 'NONE', #3080, .T. ) ;
#7639 = ORIENTED_EDGE ( 'NONE', *, *, #11976, .T. ) ;
#7640 = AXIS2_PLACEMENT_3D ( 'NONE', #10182, #4391, #12136 ) ;
#7641 = EDGE_CURVE ( 'NONE', #12030, #11226, #1451, .T. ) ;
#7642 = ADVANCED_FACE ( 'NONE', ( #2900, #4834 ), #3838, .F. ) ;
#7643 = APPLICATION_CONTEXT ( 'automotive_design' ) ;
#7644 = EDGE_CURVE ( 'NONE', #9024, #7513, #8402, .T. ) ;
#7645 = CARTESIAN_POINT ( 'NONE',  ( 70.82643617010577941, 41.06116477461475966, -24.89585111361949643 ) ) ;
#7646 =( NAMED_UNIT ( * ) PLANE_ANGLE_UNIT ( ) SI_UNIT ( $, .RADIAN. ) );
#7647 = DIRECTION ( 'NONE',  ( 0.000000000000000000, 1.000000000000000000, 0.000000000000000000 ) ) ;
#7648 = AXIS2_PLACEMENT_3D ( 'NONE', #5575, #1016, #3883 ) ;
#7649 = CARTESIAN_POINT ( 'NONE',  ( 140.0000000000011369, 225.0000000000000853, -20.00000000000000000 ) ) ;
#7650 = CARTESIAN_POINT ( 'NONE',  ( 2.143131898507868248E-15, 122.0000000000000000, 17.50000000000000000 ) ) ;
#7651 = CARTESIAN_POINT ( 'NONE',  ( 71.74731260882261097, 15.26788291291094168, -21.96902955818390168 ) ) ;
#7652 = ORIENTED_EDGE ( 'NONE', *, *, #6127, .F. ) ;
#7653 = CARTESIAN_POINT ( 'NONE',  ( -3.250000000000000444, 111.4375000000000000, 1.346194077712559167 ) ) ;
#7654 = CARTESIAN_POINT ( 'NONE',  ( -2.708734125000000326, 110.7499999986343937, 1.121994411437818862 ) ) ;
#7655 = ORIENTED_EDGE ( 'NONE', *, *, #11767, .F. ) ;
#7656 = DIRECTION ( 'NONE',  ( 0.000000000000000000, 1.000000000000000000, 0.000000000000000000 ) ) ;
#7657 = AXIS2_PLACEMENT_3D ( 'NONE', #7473, #8269, #5543 ) ;
#7658 = EDGE_LOOP ( 'NONE', ( #10590, #7078, #5645, #8560 ) ) ;
#7659 = LINE ( 'NONE', #7540, #5154 ) ;
#7660 = CARTESIAN_POINT ( 'NONE',  ( 0.000000000000000000, 127.0000000000000000, 0.000000000000000000 ) ) ;
#7661 = ORIENTED_EDGE ( 'NONE', *, *, #10586, .F. ) ;
#7662 = CARTESIAN_POINT ( 'NONE',  ( 30.07733313487553772, 77.00000000000709122, -4.660254037819535178 ) ) ;
#7663 = CARTESIAN_POINT ( 'NONE',  ( 27.31068353816013783, 86.91310272383458368, 12.41479448187959278 ) ) ;
#7664 = ORIENTED_EDGE ( 'NONE', *, *, #3001, .T. ) ;
#7665 = ITEM_DEFINED_TRANSFORMATION ( 'NONE', 'NONE', #5950,  #1612 ) ;
#7666 = LINE ( 'NONE', #7790, #9220 ) ;
#7667 = VECTOR ( 'NONE', #1382, 1000.000000000000000 ) ;
#7668 = DIRECTION ( 'NONE',  ( -1.000000000000000000, 0.000000000000000000, -0.000000000000000000 ) ) ;
#7669 = DIRECTION ( 'NONE',  ( 0.000000000000000000, 0.000000000000000000, 1.000000000000000000 ) ) ;
#7670 = ORIENTED_EDGE ( 'NONE', *, *, #832, .T. ) ;
#7671 = CARTESIAN_POINT ( 'NONE',  ( -1.121994411437820416, 110.9999999986343937, -2.708734124999999882 ) ) ;
#7672 = LINE ( 'NONE', #10413, #6969 ) ;
#7673 = EDGE_CURVE ( 'NONE', #7980, #8527, #11810, .T. ) ;
#7674 = AXIS2_PLACEMENT_3D ( 'NONE', #12188, #3635, #2823 ) ;
#7675 = ORIENTED_EDGE ( 'NONE', *, *, #7715, .T. ) ;
#7676 = PLANE ( 'NONE',  #7362 ) ;
#7677 = CARTESIAN_POINT ( 'NONE',  ( -7.076627832483614711, 16.19342887763680494, 74.66686486294869951 ) ) ;
#7678 = CLOSED_SHELL ( 'NONE', ( #7373, #5046, #5443, #3513, #6388, #5922, #2596, #10693, #9109, #8609, #2550, #3804, #6194, #11655, #11853, #10430, #7905, #8981, #3814, #10658, #5029, #9161, #11146, #476, #717, #4450, #3500, #6983, #8448, #5345, #1835, #3731, #9949, #12118, #5752, #7985, #10490, #2569, #12326, #7153, #10340, #1553, #8220, #8822, #1433, #4329, #377, #3132, #1051, #1639, #6097, #295, #10722, #1871, #6156, #11189, #8629, #9408, #11378, #10196, #4195, #10154, #7699, #5918, #4061, #11570 ) ) ;
#7679 = VERTEX_POINT ( 'NONE', #5652 ) ;
#7680 = FACE_OUTER_BOUND ( 'NONE', #3441, .T. ) ;
#7681 = CARTESIAN_POINT ( 'NONE',  ( 138.5355339059338462, 63.53553390593273775, 20.00000000000000000 ) ) ;
#7682 = VERTEX_POINT ( 'NONE', #4704 ) ;
#7683 = LINE ( 'NONE', #9723, #1309 ) ;
#7684 = FACE_OUTER_BOUND ( 'NONE', #5133, .T. ) ;
#7685 = FACE_OUTER_BOUND ( 'NONE', #8918, .T. ) ;
#7686 = AXIS2_PLACEMENT_3D ( 'NONE', #6430, #5434, #8221 ) ;
#7687 = DIRECTION ( 'NONE',  ( 0.000000000000000000, 0.000000000000000000, 1.000000000000000000 ) ) ;
#7688 = CARTESIAN_POINT ( 'NONE',  ( -1.346194077712559389, 112.3125000000000000, 3.250000000000000444 ) ) ;
#7689 = ADVANCED_FACE ( 'NONE', ( #6705 ), #10796, .F. ) ;
#7690 = CARTESIAN_POINT ( 'NONE',  ( 72.45961080413260902, 10.00000000123442412, 19.36513408292344351 ) ) ;
#7691 = EDGE_CURVE ( 'NONE', #1251, #632, #7758, .T. ) ;
#7692 = FILL_AREA_STYLE_COLOUR ( '', #11117 ) ;
#7693 = ORIENTED_EDGE ( 'NONE', *, *, #8127, .T. ) ;
#7694 = DIRECTION ( 'NONE',  ( -0.000000000000000000, 1.000000000000000000, -0.000000000000000000 ) ) ;
#7695 = FACE_BOUND ( 'NONE', #2669, .T. ) ;
#7696 = ORIENTED_EDGE ( 'NONE', *, *, #2019, .F. ) ;
#7697 = CARTESIAN_POINT ( 'NONE',  ( 0.000000000000000000, 87.00000000000000000, 0.000000000000000000 ) ) ;
#7698 = LINE ( 'NONE', #11512, #6781 ) ;
#7699 = ADVANCED_FACE ( 'NONE', ( #3902 ), #6761, .T. ) ;
#7700 = AXIS2_PLACEMENT_3D ( 'NONE', #8672, #4690, #5702 ) ;
#7701 =( LENGTH_UNIT ( ) NAMED_UNIT ( * ) SI_UNIT ( .MILLI., .METRE. ) );
#7702 = CARTESIAN_POINT ( 'NONE',  ( 0.000000000000000000, 115.0000000000000142, 0.000000000000000000 ) ) ;
#7703 = VERTEX_POINT ( 'NONE', #3025 ) ;
#7704 = EDGE_CURVE ( 'NONE', #5602, #1941, #9679, .T. ) ;
#7705 = ADVANCED_FACE ( 'NONE', ( #4960 ), #2030, .T. ) ;
#7706 = FILL_AREA_STYLE ('',( #8627 ) ) ;
#7707 = EDGE_LOOP ( 'NONE', ( #1193, #1317 ) ) ;
#7708 = CARTESIAN_POINT ( 'NONE',  ( 75.47338808840343916, 43.79030468642783092, -23.26499062814251317 ) ) ;
#7709 = SURFACE_STYLE_FILL_AREA ( #3780 ) ;
#7710 = LINE ( 'NONE', #5785, #2065 ) ;
#7711 = DIRECTION ( 'NONE',  ( 0.000000000000000000, 1.000000000000000000, 0.000000000000000000 ) ) ;
#7712 = CARTESIAN_POINT ( 'NONE',  ( 20.00000000000000355, 7.965803112215716020, -57.08203932499370836 ) ) ;
#7713 = CARTESIAN_POINT ( 'NONE',  ( 75.47443053502085775, 16.20845120114963933, -23.26350036030322954 ) ) ;
#7714 = ORIENTED_EDGE ( 'NONE', *, *, #5096, .F. ) ;
#7715 = EDGE_CURVE ( 'NONE', #357, #11448, #7019, .T. ) ;
#7716 = DIRECTION ( 'NONE',  ( 0.000000000000000000, -0.000000000000000000, 1.000000000000000000 ) ) ;
#7717 = DIRECTION ( 'NONE',  ( -0.000000000000000000, 1.000000000000000000, -0.000000000000000000 ) ) ;
#7718 = ORIENTED_EDGE ( 'NONE', *, *, #7802, .T. ) ;
#7719 = FACE_OUTER_BOUND ( 'NONE', #5491, .T. ) ;
#7720 = AXIS2_PLACEMENT_3D ( 'NONE', #1626, #10211, #6488 ) ;
#7721 = EDGE_LOOP ( 'NONE', ( #11046, #8727, #2849, #372, #11284, #139, #168, #11735, #2296, #9907, #3830, #919, #11580, #1101, #1161, #5917, #3239, #7189, #3109, #3059, #7908, #11921, #1012, #2757, #5559, #12110, #10782, #9292, #7574, #2450, #8574, #11602, #5130 ) ) ;
#7722 = CARTESIAN_POINT ( 'NONE',  ( 1.285879139104721107E-14, 335.0000000000000000, -105.0000000000000284 ) ) ;
#7723 = CARTESIAN_POINT ( 'NONE',  ( 75.70364277637114014, 44.05991784979070047, 22.93512150616605538 ) ) ;
#7724 = ORIENTED_EDGE ( 'NONE', *, *, #5795, .F. ) ;
#7725 = CARTESIAN_POINT ( 'NONE',  ( 0.000000000000000000, 87.00000000000000000, -25.50000000000000000 ) ) ;
#7726 = EDGE_CURVE ( 'NONE', #2243, #7094, #8198, .T. ) ;
#7727 = CARTESIAN_POINT ( 'NONE',  ( -1.440781129305282571, 17.00240406844413243, 80.00000000000000000 ) ) ;
#7728 = ORIENTED_EDGE ( 'NONE', *, *, #4389, .F. ) ;
#7729 = APPLICATION_PROTOCOL_DEFINITION ( 'draft international standard', 'automotive_design', 1998, #9946 ) ;
#7730 = CARTESIAN_POINT ( 'NONE',  ( 11.80921887069467324, 29.91666666666539953, 80.00000000000000000 ) ) ;
#7731 = CARTESIAN_POINT ( 'NONE',  ( 20.00000000000000711, 63.00000000000000000, 67.08203932499370126 ) ) ;
#7732 = CARTESIAN_POINT ( 'NONE',  ( 3.592712519748450628, 38.78525403784453118, 79.50000000000000000 ) ) ;
#7733 = AXIS2_PLACEMENT_3D ( 'NONE', #5128, #8904, #6175 ) ;
#7734 = VERTEX_POINT ( 'NONE', #146 ) ;
#7735 = CARTESIAN_POINT ( 'NONE',  ( 1.121994411437818862, 113.4999999986344079, 2.708734125000000326 ) ) ;
#7736 = CARTESIAN_POINT ( 'NONE',  ( -2.298097038856279806, 112.4999999972688158, -2.298097038856279362 ) ) ;
#7737 = ORIENTED_EDGE ( 'NONE', *, *, #9181, .T. ) ;
#7738 = DIRECTION ( 'NONE',  ( 0.000000000000000000, 1.000000000000000000, 0.000000000000000000 ) ) ;
#7739 = VERTEX_POINT ( 'NONE', #11571 ) ;
#7740 = DIRECTION ( 'NONE',  ( -0.7236679289129753778, 0.000000000000000000, 0.6901483381584025967 ) ) ;
#7741 = DIRECTION ( 'NONE',  ( -0.000000000000000000, -1.000000000000000000, -0.000000000000000000 ) ) ;
#7742 = ORIENTED_EDGE ( 'NONE', *, *, #3831, .T. ) ;
#7743 = CARTESIAN_POINT ( 'NONE',  ( -3.250000000000001776, 110.5625000000000000, -1.346194077712558279 ) ) ;
#7744 = DIRECTION ( 'NONE',  ( 0.000000000000000000, 1.000000000000000000, 0.000000000000000000 ) ) ;
#7745 = DIRECTION ( 'NONE',  ( -0.000000000000000000, -0.000000000000000000, 1.000000000000000000 ) ) ;
#7746 = EDGE_CURVE ( 'NONE', #9696, #3575, #9429, .T. ) ;
#7747 = CARTESIAN_POINT ( 'NONE',  ( -27.46866764507868908, 86.65804127256191691, -12.06796414783013027 ) ) ;
#7748 = CYLINDRICAL_SURFACE ( 'NONE', #11151, 3.250000000000000444 ) ;
#7749 = ADVANCED_FACE ( 'NONE', ( #10624 ), #5896, .F. ) ;
#7750 = CARTESIAN_POINT ( 'NONE',  ( 72.61843774138908714, 10.00000000000009059, 18.75000000000000355 ) ) ;
#7751 = AXIS2_PLACEMENT_3D ( 'NONE', #10120, #3532, #7334 ) ;
#7752 = ORIENTED_EDGE ( 'NONE', *, *, #1892, .F. ) ;
#7753 = PRODUCT_CONTEXT ( 'NONE', #641, 'mechanical' ) ;
#7754 = ORIENTED_EDGE ( 'NONE', *, *, #8075, .F. ) ;
#7755 = CARTESIAN_POINT ( 'NONE',  ( 147.9289321881356045, 20.00000000000008527, -25.00000000000000000 ) ) ;
#7756 = DIRECTION ( 'NONE',  ( 1.000000000000000000, 0.000000000000000000, 0.000000000000000000 ) ) ;
#7757 = ORIENTED_EDGE ( 'NONE', *, *, #7430, .F. ) ;
#7758 = LINE ( 'NONE', #10501, #6825 ) ;
#7759 = AXIS2_PLACEMENT_3D ( 'NONE', #5610, #9388, #3727 ) ;
#7760 = CARTESIAN_POINT ( 'NONE',  ( -1.190781129305471087, 30.00000000000008882, 80.00000000000000000 ) ) ;
#7761 = DIRECTION ( 'NONE',  ( 0.000000000000000000, 0.000000000000000000, 1.000000000000000000 ) ) ;
#7762 = ADVANCED_FACE ( 'NONE', ( #8745, #7820 ), #12319, .F. ) ;
#7763 = EDGE_CURVE ( 'NONE', #5980, #11423, #1341, .T. ) ;
#7764 = ORIENTED_EDGE ( 'NONE', *, *, #8287, .F. ) ;
#7765 = EDGE_CURVE ( 'NONE', #6973, #6185, #4320, .T. ) ;
#7766 = EDGE_CURVE ( 'NONE', #2602, #7317, #4230, .T. ) ;
#7767 = LINE ( 'NONE', #1975, #10015 ) ;
#7768 = CARTESIAN_POINT ( 'NONE',  ( 0.000000000000000000, 87.00000000000000000, 0.000000000000000000 ) ) ;
#7769 = VERTEX_POINT ( 'NONE', #8806 ) ;
#7770 = DIRECTION ( 'NONE',  ( -0.000000000000000000, 1.000000000000000000, -0.000000000000000000 ) ) ;
#7771 = CARTESIAN_POINT ( 'NONE',  ( 70.92186449036606177, 12.01005621119159450, -24.39573567383822095 ) ) ;
#7772 = ORIENTED_EDGE ( 'NONE', *, *, #1760, .T. ) ;
#7773 = CARTESIAN_POINT ( 'NONE',  ( -2.298097038856279806, 111.6250000000000000, -2.298097038856279362 ) ) ;
#7774 = VECTOR ( 'NONE', #1762, 1000.000000000000000 ) ;
#7775 = FACE_OUTER_BOUND ( 'NONE', #571, .T. ) ;
#7776 = ORIENTED_EDGE ( 'NONE', *, *, #3705, .F. ) ;
#7777 = CARTESIAN_POINT ( 'NONE',  ( -17.30235457177319347, 275.0000000000000000, -113.6909342308024549 ) ) ;
#7778 = VECTOR ( 'NONE', #9619, 1000.000000000000000 ) ;
#7779 = AXIS2_PLACEMENT_3D ( 'NONE', #704, #11362, #4436 ) ;
#7780 = PRODUCT_DEFINITION ( 'UNKNOWN', '', #7924, #6014 ) ;
#7781 = ORIENTED_EDGE ( 'NONE', *, *, #7154, .F. ) ;
#7782 = CARTESIAN_POINT ( 'NONE',  ( 5.525725221640833240, 18.86666975080242992, 80.00000000000000000 ) ) ;
#7783 = DIRECTION ( 'NONE',  ( -0.000000000000000000, -0.000000000000000000, 1.000000000000000000 ) ) ;
#7784 = ORIENTED_EDGE ( 'NONE', *, *, #10258, .F. ) ;
#7785 = CARTESIAN_POINT ( 'NONE',  ( 24.76446302067270722, 275.0000000000000000, -102.0378428393002679 ) ) ;
#7786 = LINE ( 'NONE', #1127, #11076 ) ;
#7787 = ORIENTED_EDGE ( 'NONE', *, *, #11055, .T. ) ;
#7788 = AXIS2_PLACEMENT_3D ( 'NONE', #5880, #11619, #7238 ) ;
#7789 = PRODUCT_CONTEXT ( 'NONE', #3181, 'mechanical' ) ;
#7790 = CARTESIAN_POINT ( 'NONE',  ( 2.500000000000000000, 2.500728763858895382E-16, -2.041999999999999815 ) ) ;
#7791 = VECTOR ( 'NONE', #2996, 1000.000000000000114 ) ;
#7792 = CARTESIAN_POINT ( 'NONE',  ( 3.245314017740478073E-16, 165.5000000000000000, -2.649999999999993694 ) ) ;
#7793 = EDGE_LOOP ( 'NONE', ( #9334, #1407, #3851, #10681 ) ) ;
#7794 = CARTESIAN_POINT ( 'NONE',  ( 150.0000000000010800, 15.00000000000008882, 20.00000000000000000 ) ) ;
#7795 = DIRECTION ( 'NONE',  ( 7.011174048739587977E-15, 1.000000000000000000, 0.000000000000000000 ) ) ;
#7796 = EDGE_CURVE ( 'NONE', #4313, #4047, #11208, .T. ) ;
#7797 = ADVANCED_FACE ( 'NONE', ( #6018 ), #8055, .F. ) ;
#7798 = VECTOR ( 'NONE', #4152, 1000.000000000000000 ) ;
#7799 = CIRCLE ( 'NONE', #1630, 5.000000000000000000 ) ;
#7800 = ORIENTED_EDGE ( 'NONE', *, *, #8367, .T. ) ;
#7801 = CARTESIAN_POINT ( 'NONE',  ( 145.0000000000011369, 225.0000000000000853, -20.00000000000000000 ) ) ;
#7802 = EDGE_CURVE ( 'NONE', #1278, #2816, #12209, .T. ) ;
#7803 = CARTESIAN_POINT ( 'NONE',  ( 1.088204915335219061E-15, 15.04734002586538821, 75.00000000000001421 ) ) ;
#7804 = ORIENTED_EDGE ( 'NONE', *, *, #7605, .T. ) ;
#7805 = DIRECTION ( 'NONE',  ( -1.000000000000000000, 0.000000000000000000, 0.000000000000000000 ) ) ;
#7806 = CARTESIAN_POINT ( 'NONE',  ( 69.55717041450677129, 18.69586594910642319, 28.04997484771492466 ) ) ;
#7807 = ORIENTED_EDGE ( 'NONE', *, *, #8037, .T. ) ;
#7808 = CARTESIAN_POINT ( 'NONE',  ( -30.00100000000000122, 87.00000000000000000, 8.660254037844435260 ) ) ;
#7809 = LINE ( 'NONE', #11623, #6912 ) ;
#7810 = CARTESIAN_POINT ( 'NONE',  ( -0.9407811293052614765, 20.00000000000009237, 79.50000000000000000 ) ) ;
#7811 = DIRECTION ( 'NONE',  ( 0.000000000000000000, 0.000000000000000000, -1.000000000000000000 ) ) ;
#7812 = DIRECTION ( 'NONE',  ( -0.000000000000000000, -1.000000000000000000, -0.000000000000000000 ) ) ;
#7813 = AXIS2_PLACEMENT_3D ( 'NONE', #1399, #2330, #5208 ) ;
#7814 = CARTESIAN_POINT ( 'NONE',  ( 1.658621287961228320E-16, 113.8124999986344079, 2.708734124999999882 ) ) ;
#7815 = VERTEX_POINT ( 'NONE', #8989 ) ;
#7816 = ORIENTED_EDGE ( 'NONE', *, *, #2291, .T. ) ;
#7817 = DIRECTION ( 'NONE',  ( -0.000000000000000000, -1.000000000000000000, -0.000000000000000000 ) ) ;
#7818 = CARTESIAN_POINT ( 'NONE',  ( 1.850901974874337830, 44.71779529743732695, 74.98253729624308050 ) ) ;
#7819 = ORIENTED_EDGE ( 'NONE', *, *, #3331, .T. ) ;
#7820 = FACE_OUTER_BOUND ( 'NONE', #7155, .T. ) ;
#7821 = CARTESIAN_POINT ( 'NONE',  ( -1.440781129305471087, 43.00000000000008527, 79.50000000000000000 ) ) ;
#7822 = CARTESIAN_POINT ( 'NONE',  ( 2.708734125000000326, 110.3749999986344079, 1.121994411437819084 ) ) ;
#7823 = DIRECTION ( 'NONE',  ( 0.000000000000000000, 0.000000000000000000, 1.000000000000000000 ) ) ;
#7824 = ORIENTED_EDGE ( 'NONE', *, *, #11486, .T. ) ;
#7825 = VECTOR ( 'NONE', #2417, 1000.000000000000000 ) ;
#7826 = EDGE_CURVE ( 'NONE', #5730, #381, #4262, .T. ) ;
#7827 =( NAMED_UNIT ( * ) PLANE_ANGLE_UNIT ( ) SI_UNIT ( $, .RADIAN. ) );
#7828 = CYLINDRICAL_SURFACE ( 'NONE', #1854, 15.00000000000000000 ) ;
#7829 = DIRECTION ( 'NONE',  ( 0.000000000000000000, 1.000000000000000000, 0.000000000000000000 ) ) ;
#7830 = ORIENTED_EDGE ( 'NONE', *, *, #10765, .F. ) ;
#7831 = CARTESIAN_POINT ( 'NONE',  ( 77.11786746747833377, 15.03129260902921516, -20.64504863446460803 ) ) ;
#7832 = AXIS2_PLACEMENT_3D ( 'NONE', #9444, #11280, #4535 ) ;
#7833 = CARTESIAN_POINT ( 'NONE',  ( -5.970153145843347347E-16, 111.7500000000000000, -3.250000000000000444 ) ) ;
#7834 = FACE_OUTER_BOUND ( 'NONE', #9678, .T. ) ;
#7835 = ORIENTED_EDGE ( 'NONE', *, *, #9592, .F. ) ;
#7836 = CARTESIAN_POINT ( 'NONE',  ( 5.525725221640672480, 41.13333024919784719, 79.50000000000000000 ) ) ;
#7837 = EDGE_CURVE ( 'NONE', #8588, #10191, #11822, .T. ) ;
#7838 = TOROIDAL_SURFACE ( 'NONE', #9219, 10.00000000000000000, 5.000000000000000000 ) ;
#7839 = VERTEX_POINT ( 'NONE', #335 ) ;
#7840 = LINE ( 'NONE', #533, #5350 ) ;
#7841 = CARTESIAN_POINT ( 'NONE',  ( 120.0000000000010090, 45.00000000000009237, -20.00000000000000000 ) ) ;
#7842 = ORIENTED_EDGE ( 'NONE', *, *, #10645, .F. ) ;
#7843 = LINE ( 'NONE', #10712, #2490 ) ;
#7844 = DIRECTION ( 'NONE',  ( 0.000000000000000000, -0.000000000000000000, 1.000000000000000000 ) ) ;
#7845 = ORIENTED_EDGE ( 'NONE', *, *, #2199, .F. ) ;
#7846 = CARTESIAN_POINT ( 'NONE',  ( 0.000000000000000000, 285.0000000000000568, 0.000000000000000000 ) ) ;
#7847 = FACE_OUTER_BOUND ( 'NONE', #4451, .T. ) ;
#7848 = ORIENTED_EDGE ( 'NONE', *, *, #3045, .F. ) ;
#7849 = CARTESIAN_POINT ( 'NONE',  ( 1.121994411437819528, 112.1249999986343937, -2.708734124999999882 ) ) ;
#7850 = CIRCLE ( 'NONE', #2083, 125.0000000000000284 ) ;
#7851 = CARTESIAN_POINT ( 'NONE',  ( 1.990051048614449116E-16, 111.1249999972688158, 3.250000000000000444 ) ) ;
#7852 = VERTEX_POINT ( 'NONE', #1280 ) ;
#7853 = CARTESIAN_POINT ( 'NONE',  ( -8.500000000000000000, 165.5000000000000000, 6.164414002968973350 ) ) ;
#7854 = DIRECTION ( 'NONE',  ( -0.000000000000000000, -0.000000000000000000, 1.000000000000000000 ) ) ;
#7855 = AXIS2_PLACEMENT_3D ( 'NONE', #744, #7288, #4536 ) ;
#7856 = ORIENTED_EDGE ( 'NONE', *, *, #9336, .T. ) ;
#7857 = CIRCLE ( 'NONE', #2683, 30.00000000000000000 ) ;
#7858 = CARTESIAN_POINT ( 'NONE',  ( 2.500000000000000000, -1.178949249685214307, 2.042000000000001592 ) ) ;
#7859 = DIRECTION ( 'NONE',  ( -0.8660254037844399289, -0.4999999999999977796, 0.000000000000000000 ) ) ;
#7860 = ORIENTED_EDGE ( 'NONE', *, *, #9421, .T. ) ;
#7861 = CARTESIAN_POINT ( 'NONE',  ( 0.000000000000000000, 75.00000000000001421, -15.00000000000000000 ) ) ;
#7862 = EDGE_CURVE ( 'NONE', #10543, #4650, #4634, .T. ) ;
#7863 = FACE_OUTER_BOUND ( 'NONE', #2070, .T. ) ;
#7864 = CARTESIAN_POINT ( 'NONE',  ( 5.525725221640672480, 41.13333024919784719, 79.50000000000000000 ) ) ;
#7865 = STYLED_ITEM ( 'NONE', ( #8880 ), #543 ) ;
#7866 = ORIENTED_EDGE ( 'NONE', *, *, #9206, .F. ) ;
#7867 = CARTESIAN_POINT ( 'NONE',  ( -7.618612345655469298, 41.29999691586513677, 80.00000000000000000 ) ) ;
#7868 = CARTESIAN_POINT ( 'NONE',  ( -1.121994411437819084, 111.8749999986343937, 2.708734124999999882 ) ) ;
#7869 = AXIS2_PLACEMENT_3D ( 'NONE', #8512, #2916, #1977 ) ;
#7870 = ORIENTED_EDGE ( 'NONE', *, *, #9304, .T. ) ;
#7871 = ORIENTED_EDGE ( 'NONE', *, *, #4668, .F. ) ;
#7872 = PRODUCT_DEFINITION_SHAPE ( 'NONE', 'NONE',  #3674 ) ;
#7873 = DIRECTION ( 'NONE',  ( -0.000000000000000000, -1.000000000000000000, -0.000000000000000000 ) ) ;
#7874 = CARTESIAN_POINT ( 'NONE',  ( 11.02221580535522172, 38.75872166009053643, 74.18734971499729625 ) ) ;
#7875 = EDGE_LOOP ( 'NONE', ( #1436, #4361, #3520, #11445 ) ) ;
#7876 = DIRECTION ( 'NONE',  ( 0.000000000000000000, 0.000000000000000000, -1.000000000000000000 ) ) ;
#7877 = AXIS2_PLACEMENT_3D ( 'NONE', #6703, #144, #1155 ) ;
#7878 = CARTESIAN_POINT ( 'NONE',  ( 27.67899820261485999, 88.38261385519929547, 11.05501148229834030 ) ) ;
#7879 = DIRECTION ( 'NONE',  ( 0.000000000000000000, 1.000000000000000000, 0.000000000000000000 ) ) ;
#7880 = DIRECTION ( 'NONE',  ( 2.213536252433181319E-16, 0.000000000000000000, 1.000000000000000000 ) ) ;
#7881 = TOROIDAL_SURFACE ( 'NONE', #10860, 65.00000000000001421, 5.000000000000000000 ) ;
#7882 = VERTEX_POINT ( 'NONE', #1463 ) ;
#7883 = AXIS2_PLACEMENT_3D ( 'NONE', #12083, #6401, #10188 ) ;
#7884 = CARTESIAN_POINT ( 'NONE',  ( -116.4243635975518742, 275.0000000000000000, 45.50129185973785440 ) ) ;
#7885 = CYLINDRICAL_SURFACE ( 'NONE', #3061, 15.00000000000000000 ) ;
#7886 = PLANE ( 'NONE',  #11593 ) ;
#7887 = DIRECTION ( 'NONE',  ( 0.8660254037844331565, -0.5000000000000095479, 0.000000000000000000 ) ) ;
#7888 = CARTESIAN_POINT ( 'NONE',  ( 72.54053945714667861, 14.91954699701732423, -19.05169875840561389 ) ) ;
#7889 = DIRECTION ( 'NONE',  ( -0.000000000000000000, -1.000000000000000000, -0.000000000000000000 ) ) ;
#7890 = CARTESIAN_POINT ( 'NONE',  ( 1.915364268218909594, 111.4374999986344079, 1.915364268218909594 ) ) ;
#7891 = EDGE_CURVE ( 'NONE', #381, #5735, #11606, .T. ) ;
#7892 = EDGE_LOOP ( 'NONE', ( #8331, #10410, #7555, #8159 ) ) ;
#7893 = LINE ( 'NONE', #11653, #1408 ) ;
#7894 = VECTOR ( 'NONE', #2825, 1000.000000000000000 ) ;
#7895 = EDGE_CURVE ( 'NONE', #6417, #9081, #4203, .T. ) ;
#7896 = ORIENTED_EDGE ( 'NONE', *, *, #2806, .T. ) ;
#7897 = PLANE ( 'NONE',  #9200 ) ;
#7898 = VERTEX_POINT ( 'NONE', #7932 ) ;
#7899 = CARTESIAN_POINT ( 'NONE',  ( 34.77260134704101802, 76.42358343581042845, -8.327459779344241753 ) ) ;
#7900 = DIRECTION ( 'NONE',  ( 0.000000000000000000, 0.000000000000000000, 1.000000000000000000 ) ) ;
#7901 = ORIENTED_EDGE ( 'NONE', *, *, #5402, .T. ) ;
#7902 = CARTESIAN_POINT ( 'NONE',  ( 0.000000000000000000, 75.00000000000001421, 25.00000000000000000 ) ) ;
#7903 =( BOUNDED_CURVE ( )  B_SPLINE_CURVE ( 2, ( #7537, #6371, #5504, #10159, #4500 ),
 .UNSPECIFIED., .F., .F. ) 
 B_SPLINE_CURVE_WITH_KNOTS ( ( 3, 2, 3 ),
 ( 0.000000000000000000, 0.03125000000000002776, 0.06250000000000005551 ),
 .UNSPECIFIED. ) 
 CURVE ( )  GEOMETRIC_REPRESENTATION_ITEM ( )  RATIONAL_B_SPLINE_CURVE ( ( 1.000000000000000000, 0.9238795325112867385, 1.000000000000000000, 0.9238795325112866275, 1.000000000000000222 ) ) 
 REPRESENTATION_ITEM ( '' )  );
#7904 = CARTESIAN_POINT ( 'NONE',  ( 8.939921633775681592E-15, 67.00000000000000000, 73.00000000000002842 ) ) ;
#7905 = ADVANCED_FACE ( 'NONE', ( #5269 ), #10869, .F. ) ;
#7906 = ORIENTED_EDGE ( 'NONE', *, *, #200, .T. ) ;
#7907 = CARTESIAN_POINT ( 'NONE',  ( 2.708734125000000326, 113.3124999986344079, 0.000000000000000000 ) ) ;
#7908 = ORIENTED_EDGE ( 'NONE', *, *, #3662, .F. ) ;
#7909 = CARTESIAN_POINT ( 'NONE',  ( 31.00813199677072873, 87.06416249055504863, 8.771386731425977246 ) ) ;
#7910 = CARTESIAN_POINT ( 'NONE',  ( -10.61565724859829096, 18.28584071866657013, 74.24882261665963767 ) ) ;
#7911 = EDGE_LOOP ( 'NONE', ( #4243, #815, #8875, #5539, #15 ) ) ;
#7912 = DIRECTION ( 'NONE',  ( -0.000000000000000000, 1.000000000000000000, -0.000000000000000000 ) ) ;
#7913 = CARTESIAN_POINT ( 'NONE',  ( 71.75867793008815454, 10.54280999270224406, 21.81257403104604720 ) ) ;
#7914 = CIRCLE ( 'NONE', #3349, 25.50000000000000000 ) ;
#7915 = ORIENTED_EDGE ( 'NONE', *, *, #6347, .F. ) ;
#7916 = EDGE_CURVE ( 'NONE', #1468, #3039, #1522, .T. ) ;
#7917 = ADVANCED_FACE ( 'NONE', ( #11756 ), #9927, .T. ) ;
#7918 = LINE ( 'NONE', #7117, #2858 ) ;
#7919 = CARTESIAN_POINT ( 'NONE',  ( 74.19409830870891653, 40.72200583775279625, -24.96047248796921281 ) ) ;
#7920 = LINE ( 'NONE', #11501, #10566 ) ;
#7921 = ORIENTED_EDGE ( 'NONE', *, *, #6984, .F. ) ;
#7922 = DIRECTION ( 'NONE',  ( 0.000000000000000000, 0.000000000000000000, 1.000000000000000000 ) ) ;
#7923 = CARTESIAN_POINT ( 'NONE',  ( 74.58430552652164636, 17.74813588577157475, 24.46729545492024016 ) ) ;
#7924 = PRODUCT_DEFINITION_FORMATION_WITH_SPECIFIED_SOURCE ( 'ANY', '', #1899, .NOT_KNOWN. ) ;
#7925 = ORIENTED_EDGE ( 'NONE', *, *, #433, .F. ) ;
#7926 = FACE_OUTER_BOUND ( 'NONE', #3192, .T. ) ;
#7927 = CARTESIAN_POINT ( 'NONE',  ( 71.89703483713221033, 44.94224125782246659, -21.44956398270095121 ) ) ;
#7928 = VERTEX_POINT ( 'NONE', #9048 ) ;
#7929 = LINE ( 'NONE', #2086, #2475 ) ;
#7930 = CARTESIAN_POINT ( 'NONE',  ( 72.14031151490229377, 45.12527760491855844, 20.56889282980839440 ) ) ;
#7931 = VERTEX_POINT ( 'NONE', #10747 ) ;
#7932 = CARTESIAN_POINT ( 'NONE',  ( -109.9268209223825750, 275.0000000000000000, 32.26598893414599445 ) ) ;
#7933 = CARTESIAN_POINT ( 'NONE',  ( -2.298097038856279806, 112.4999999972688158, -2.298097038856279362 ) ) ;
#7934 = FACE_OUTER_BOUND ( 'NONE', #11865, .T. ) ;
#7935 = EDGE_LOOP ( 'NONE', ( #3694, #5516, #4296, #296, #7776 ) ) ;
#7936 = VERTEX_POINT ( 'NONE', #2209 ) ;
#7937 = SURFACE_STYLE_FILL_AREA ( #342 ) ;
#7938 = ADVANCED_FACE ( 'NONE', ( #9867 ), #7993, .T. ) ;
#7939 = CIRCLE ( 'NONE', #9532, 2.000000000000001776 ) ;
#7940 = VECTOR ( 'NONE', #1578, 1000.000000000000000 ) ;
#7941 = CARTESIAN_POINT ( 'NONE',  ( 25.00000000000000000, 445.0000000000000568, -59.99999999999999289 ) ) ;
#7943 = EDGE_CURVE ( 'NONE', #3197, #8944, #651, .T. ) ;
#7942 = CARTESIAN_POINT ( 'NONE',  ( -9.726035167149728267, 35.21650635094616888, 80.00000000000000000 ) ) ;
#7944 = CARTESIAN_POINT ( 'NONE',  ( 23.42809864819168553, 58.42809864819167132, -66.05997777686947359 ) ) ;
#7945 = FILL_AREA_STYLE ('',( #11706 ) ) ;
#7946 = LINE ( 'NONE', #8941, #8476 ) ;
#7947 = CARTESIAN_POINT ( 'NONE',  ( 25.00000000000000000, 570.2996408614167194, -90.00000000000000000 ) ) ;
#7948 = CARTESIAN_POINT ( 'NONE',  ( -2.298097038856279362, 110.3750000000000000, 2.298097038856279806 ) ) ;
#7949 = VECTOR ( 'NONE', #8854, 999.9999999999998863 ) ;
#7950 = VERTEX_POINT ( 'NONE', #10051 ) ;
#7951 = CARTESIAN_POINT ( 'NONE',  ( 10.19254911989230727, 36.28349364905406560, 79.50000000000000000 ) ) ;
#7952 = VECTOR ( 'NONE', #7565, 1000.000000000000000 ) ;
#7953 = ADVANCED_FACE ( 'NONE', ( #10473 ), #9389, .F. ) ;
#7954 = ORIENTED_EDGE ( 'NONE', *, *, #9074, .F. ) ;
#7955 = VECTOR ( 'NONE', #11530, 1000.000000000000114 ) ;
#7956 = CARTESIAN_POINT ( 'NONE',  ( 5.092712519748452848, 41.38333024919784719, 80.00000000000000000 ) ) ;
#7957 = EDGE_LOOP ( 'NONE', ( #4006, #7742, #9487, #6595 ) ) ;
#7958 = FACE_OUTER_BOUND ( 'NONE', #1052, .T. ) ;
#7959 = CARTESIAN_POINT ( 'NONE',  ( 1.836970198721029589E-15, 75.00000000000001421, 15.00000000000000000 ) ) ;
#7960 = ORIENTED_EDGE ( 'NONE', *, *, #11113, .F. ) ;
#7961 = CARTESIAN_POINT ( 'NONE',  ( 27.30107202361637775, 86.87046582918780757, 12.43589427268144831 ) ) ;
#7962 = CARTESIAN_POINT ( 'NONE',  ( 0.2500000000000002220, 0.000000000000000000, 0.000000000000000000 ) ) ;
#7963 = ORIENTED_EDGE ( 'NONE', *, *, #3169, .F. ) ;
#7964 = CARTESIAN_POINT ( 'NONE',  ( -7.474274778359198734, 41.38333024919781167, 79.50000000000000000 ) ) ;
#7965 = AXIS2_PLACEMENT_3D ( 'NONE', #4144, #8929, #7761 ) ;
#7966 = ORIENTED_EDGE ( 'NONE', *, *, #10617, .F. ) ;
#7967 = VERTEX_POINT ( 'NONE', #12002 ) ;
#7968 = AXIS2_PLACEMENT_3D ( 'NONE', #8907, #11495, #9602 ) ;
#7969 = EDGE_CURVE ( 'NONE', #3197, #4078, #10999, .T. ) ;
#7970 = FACE_OUTER_BOUND ( 'NONE', #3691, .T. ) ;
#7971 = FACE_OUTER_BOUND ( 'NONE', #5335, .T. ) ;
#7972 = VERTEX_POINT ( 'NONE', #5389 ) ;
#7973 = CYLINDRICAL_SURFACE ( 'NONE', #5212, 5.000000000000000888 ) ;
#7974 = LINE ( 'NONE', #9786, #10470 ) ;
#7975 = CIRCLE ( 'NONE', #5805, 105.0000000000000284 ) ;
#7976 = ORIENTED_EDGE ( 'NONE', *, *, #761, .F. ) ;
#7977 = PLANE ( 'NONE',  #1299 ) ;
#7978 = CARTESIAN_POINT ( 'NONE',  ( 77.29385721799278031, 45.00000000000009237, -20.32108911529004303 ) ) ;
#7979 = FACE_OUTER_BOUND ( 'NONE', #1864, .T. ) ;
#7980 = VERTEX_POINT ( 'NONE', #3458 ) ;
#7981 = DIRECTION ( 'NONE',  ( -0.000000000000000000, 1.000000000000000000, -0.000000000000000000 ) ) ;
#7982 = CIRCLE ( 'NONE', #8784, 4.000000000000000000 ) ;
#7983 = CARTESIAN_POINT ( 'NONE',  ( 71.30804307394105024, 16.23735240717352468, 23.42323195207305986 ) ) ;
#7984 = CIRCLE ( 'NONE', #429, 5.000000000000000888 ) ;
#7985 = ADVANCED_FACE ( 'NONE', ( #7603 ), #7384, .F. ) ;
#7986 = EDGE_CURVE ( 'NONE', #9490, #10391, #6385, .T. ) ;
#7987 = ORIENTED_EDGE ( 'NONE', *, *, #4420, .F. ) ;
#7988 = CARTESIAN_POINT ( 'NONE',  ( 75.53289395085349156, 16.12981783768338673, 23.18166983250910818 ) ) ;
#7989 = DIRECTION ( 'NONE',  ( -1.000000000000000000, -0.000000000000000000, -0.000000000000000000 ) ) ;
#7990 = VERTEX_POINT ( 'NONE', #9106 ) ;
#7991 = LINE ( 'NONE', #6015, #12236 ) ;
#7992 = ORIENTED_EDGE ( 'NONE', *, *, #2906, .F. ) ;
#7993 = CYLINDRICAL_SURFACE ( 'NONE', #7813, 40.00000000000000000 ) ;
#7994 = DIRECTION ( 'NONE',  ( -0.000000000000000000, -1.000000000000000000, -0.000000000000000000 ) ) ;
#7995 =( LENGTH_UNIT ( ) NAMED_UNIT ( * ) SI_UNIT ( .MILLI., .METRE. ) );
#7996 = CARTESIAN_POINT ( 'NONE',  ( 1.915364268218908927, 112.1874999986344079, -1.915364268218909816 ) ) ;
#7997 = ORIENTED_EDGE ( 'NONE', *, *, #4145, .F. ) ;
#7998 =( BOUNDED_CURVE ( )  B_SPLINE_CURVE ( 3, ( #12011, #3467, #730, #8374 ),
 .UNSPECIFIED., .F., .F. ) 
 B_SPLINE_CURVE_WITH_KNOTS ( ( 4, 4 ),
 ( 4.712388980384687898, 6.283185307179586232 ),
 .UNSPECIFIED. ) 
 CURVE ( )  GEOMETRIC_REPRESENTATION_ITEM ( )  RATIONAL_B_SPLINE_CURVE ( ( 1.000000000000000000, 0.8047378541243646044, 0.8047378541243646044, 1.000000000000000000 ) ) 
 REPRESENTATION_ITEM ( '' )  );
#7999 = ORIENTED_EDGE ( 'NONE', *, *, #12269, .F. ) ;
#8000 =( NAMED_UNIT ( * ) SI_UNIT ( $, .STERADIAN. ) SOLID_ANGLE_UNIT ( ) );
#8001 = ORIENTED_EDGE ( 'NONE', *, *, #5883, .F. ) ;
#8002 = AXIS2_PLACEMENT_3D ( 'NONE', #7635, #1157, #3961 ) ;
#8003 = LINE ( 'NONE', #5527, #1890 ) ;
#8004 = CARTESIAN_POINT ( 'NONE',  ( 0.000000000000000000, 335.0000000000000000, -110.0000000000000284 ) ) ;
#8005 = PLANE ( 'NONE',  #12192 ) ;
#8006 = DIRECTION ( 'NONE',  ( 1.734723475976805517E-15, -1.000000000000000000, 0.000000000000000000 ) ) ;
#8007 = CARTESIAN_POINT ( 'NONE',  ( 25.00000000000000355, 450.0000000000000568, -105.0000000000000000 ) ) ;
#8008 = APPLICATION_PROTOCOL_DEFINITION ( 'draft international standard', 'automotive_design', 1998, #10350 ) ;
#8009 = DIRECTION ( 'NONE',  ( 0.000000000000000000, 0.000000000000000000, -1.000000000000000000 ) ) ;
#8010 = ADVANCED_FACE ( 'NONE', ( #718 ), #2304, .F. ) ;
#8011 = EDGE_CURVE ( 'NONE', #4574, #1744, #4445, .T. ) ;
#8012 = CARTESIAN_POINT ( 'NONE',  ( -2.708734125000000326, 112.7499999986343937, 1.121994411437818862 ) ) ;
#8013 = VECTOR ( 'NONE', #7359, 1000.000000000000114 ) ;
#8014 = ORIENTED_EDGE ( 'NONE', *, *, #8354, .F. ) ;
#8015 = FACE_OUTER_BOUND ( 'NONE', #9875, .T. ) ;
#8016 = B_SPLINE_CURVE_WITH_KNOTS ( 'NONE', 3,
 ( #10626, #10563, #2033, #4027, #25, #5838, #5717, #1159, #3840, #2903, #3963, #10440, #11389, #11574 ),
 .UNSPECIFIED., .F., .F.,
 ( 4, 2, 2, 2, 2, 2, 4 ),
 ( 0.001978049138782353184, 0.002761379211137155940, 0.003544709283491958261, 0.004328039355846760583, 0.005111369428201563772, 0.006678029572911168416, 0.008244689717620771324 ),
 .UNSPECIFIED. ) ;
#8017 = EDGE_CURVE ( 'NONE', #1438, #3622, #8070, .T. ) ;
#8018 = ORIENTED_EDGE ( 'NONE', *, *, #2540, .F. ) ;
#8019 = LINE ( 'NONE', #5170, #3646 ) ;
#8020 = ORIENTED_EDGE ( 'NONE', *, *, #2965, .T. ) ;
#8021 = FACE_OUTER_BOUND ( 'NONE', #7707, .T. ) ;
#8022 = CARTESIAN_POINT ( 'NONE',  ( 74.75199569173395275, 17.34624747208905760, -24.25052255086779240 ) ) ;
#8023 = ORIENTED_EDGE ( 'NONE', *, *, #9686, .F. ) ;
#8024 = DIRECTION ( 'NONE',  ( 0.000000000000000000, 0.000000000000000000, -1.000000000000000000 ) ) ;
#8025 = DIRECTION ( 'NONE',  ( -1.000000000000000000, -0.000000000000000000, -0.000000000000000000 ) ) ;
#8026 = ORIENTED_EDGE ( 'NONE', *, *, #4830, .T. ) ;
#8027 = CARTESIAN_POINT ( 'NONE',  ( 70.71510656582535148, 47.48972085090039030, -24.99160257227417858 ) ) ;
#8028 = VECTOR ( 'NONE', #8373, 1000.000000000000114 ) ;
#8029 = AXIS2_PLACEMENT_3D ( 'NONE', #1571, #378, #1509 ) ;
#8030 = VERTEX_POINT ( 'NONE', #8243 ) ;
#8031 = PLANE ( 'NONE',  #767 ) ;
#8032 = DIRECTION ( 'NONE',  ( -0.000000000000000000, 1.000000000000000000, -0.000000000000000000 ) ) ;
#8033 = ORIENTED_EDGE ( 'NONE', *, *, #7315, .T. ) ;
#8034 = DIRECTION ( 'NONE',  ( 0.000000000000000000, 1.000000000000000000, 0.000000000000000000 ) ) ;
#8035 = FACE_OUTER_BOUND ( 'NONE', #6143, .T. ) ;
#8036 = EDGE_LOOP ( 'NONE', ( #890, #4751, #7311, #4680 ) ) ;
#8037 = EDGE_CURVE ( 'NONE', #1569, #7018, #10063, .T. ) ;
#8038 = CIRCLE ( 'NONE', #9628, 5.000000000000000888 ) ;
#8039 = CARTESIAN_POINT ( 'NONE',  ( -1.190781129305471087, 30.00000000000008882, 78.00000000000000000 ) ) ;
#8040 = CARTESIAN_POINT ( 'NONE',  ( 100.7495955565343451, 285.0000000000000568, 29.57226733266770680 ) ) ;
#8041 = CARTESIAN_POINT ( 'NONE',  ( 20.00000000000000000, 54.99999999999999289, -67.08203932499371547 ) ) ;
#8042 = VERTEX_POINT ( 'NONE', #1648 ) ;
#8043 = LINE ( 'NONE', #8975, #1206 ) ;
#8044 = EDGE_CURVE ( 'NONE', #10772, #5989, #2518, .T. ) ;
#8045 = CARTESIAN_POINT ( 'NONE',  ( 69.53320273752072467, 19.33188093005041353, 28.10933780299437856 ) ) ;
#8046 = AXIS2_PLACEMENT_3D ( 'NONE', #5296, #8833, #8084 ) ;
#8047 = AXIS2_PLACEMENT_3D ( 'NONE', #9101, #5384, #11056 ) ;
#8048 = EDGE_LOOP ( 'NONE', ( #839, #8946, #8694, #1495 ) ) ;
#8049 = CARTESIAN_POINT ( 'NONE',  ( 72.61843774138908714, 45.00000000000009237, -18.75000000000000355 ) ) ;
#8050 = CARTESIAN_POINT ( 'NONE',  ( -1.440781129305261477, 20.00000000000009592, 79.50000000000000000 ) ) ;
#8051 = EDGE_LOOP ( 'NONE', ( #1124, #7509, #4248, #8453, #10987 ) ) ;
#8052 = PLANE ( 'NONE',  #78 ) ;
#8053 = CARTESIAN_POINT ( 'NONE',  ( 71.74731260882261097, 44.73211708709012413, 21.96902955818388392 ) ) ;
#8054 = EDGE_LOOP ( 'NONE', ( #10682, #10643, #5857, #10367 ) ) ;
#8055 = PLANE ( 'NONE',  #3639 ) ;
#8056 = DIRECTION ( 'NONE',  ( 0.000000000000000000, -0.000000000000000000, 1.000000000000000000 ) ) ;
#8057 = DIRECTION ( 'NONE',  ( 0.000000000000000000, -1.000000000000000000, 0.000000000000000000 ) ) ;
#8058 = CARTESIAN_POINT ( 'NONE',  ( 1.658621287961228566E-16, 111.5624999986344079, 2.708734125000000326 ) ) ;
#8059 = COLOUR_RGB ( '', 0.08235294, 0.09019608, 0.10196078) ;
#8060 = ADVANCED_FACE ( 'NONE', ( #7193 ), #10996, .T. ) ;
#8061 = EDGE_CURVE ( 'NONE', #934, #6417, #2442, .T. ) ;
#8062 = EDGE_LOOP ( 'NONE', ( #8781, #1839 ) ) ;
#8063 = ORIENTED_EDGE ( 'NONE', *, *, #10812, .F. ) ;
#8064 = CIRCLE ( 'NONE', #7877, 22.00000000000000355 ) ;
#8065 = EDGE_CURVE ( 'NONE', #8042, #3955, #1315, .T. ) ;
#8066 = FACE_OUTER_BOUND ( 'NONE', #5997, .T. ) ;
#8067 = CARTESIAN_POINT ( 'NONE',  ( 8.572527594031474570E-15, 65.00000000000000000, 70.00000000000001421 ) ) ;
#8068 = DIRECTION ( 'NONE',  ( -1.000000000000000000, -0.000000000000000000, -0.000000000000000000 ) ) ;
#8069 = DIRECTION ( 'NONE',  ( 0.000000000000000000, -1.000000000000000000, 0.000000000000000000 ) ) ;
#8070 = CIRCLE ( 'NONE', #6688, 15.00000000000000000 ) ;
#8071 = CARTESIAN_POINT ( 'NONE',  ( 8.809218870694669690, 29.75000000000019540, 79.50000000000000000 ) ) ;
#8072 = DIRECTION ( 'NONE',  ( 0.000000000000000000, 1.000000000000000000, 0.000000000000000000 ) ) ;
#8073 = CARTESIAN_POINT ( 'NONE',  ( 13.70065104476912587, 28.13883518474186829, 73.73801000603624800 ) ) ;
#8074 = EDGE_CURVE ( 'NONE', #8974, #6916, #4732, .T. ) ;
#8075 = EDGE_CURVE ( 'NONE', #712, #592, #9662, .T. ) ;
#8076 = CARTESIAN_POINT ( 'NONE',  ( -13.00000000000000178, 216.0365690573663926, -7.483314773547880883 ) ) ;
#8077 = CARTESIAN_POINT ( 'NONE',  ( 1.915364268218908927, 112.1874999986344079, -1.915364268218909816 ) ) ;
#8078 = FACE_OUTER_BOUND ( 'NONE', #12001, .T. ) ;
#8079 = CARTESIAN_POINT ( 'NONE',  ( 0.000000000000000000, 275.0000000000000000, 0.000000000000000000 ) ) ;
#8080 = MECHANICAL_DESIGN_GEOMETRIC_PRESENTATION_REPRESENTATION (  '', ( #9473 ), #10876 ) ;
#8081 = ORIENTED_EDGE ( 'NONE', *, *, #9975, .T. ) ;
#8082 = CYLINDRICAL_SURFACE ( 'NONE', #2464, 100.0000000000000142 ) ;
#8083 = ORIENTED_EDGE ( 'NONE', *, *, #9181, .F. ) ;
#8084 = DIRECTION ( 'NONE',  ( 0.000000000000000000, 0.000000000000000000, 1.000000000000000000 ) ) ;
#8085 = CARTESIAN_POINT ( 'NONE',  ( 0.000000000000000000, 92.00000000000000000, 0.000000000000000000 ) ) ;
#8086 = ORIENTED_EDGE ( 'NONE', *, *, #6298, .T. ) ;
#8087 = LINE ( 'NONE', #2237, #6062 ) ;
#8088 = VECTOR ( 'NONE', #6447, 1000.000000000000000 ) ;
#8089 = DIRECTION ( 'NONE',  ( 0.9595199576812789566, 0.000000000000000000, 0.2816406412635022449 ) ) ;
#8090 = ORIENTED_EDGE ( 'NONE', *, *, #11885, .T. ) ;
#8091 = CARTESIAN_POINT ( 'NONE',  ( 72.28523001630050260, 49.93187928610722537, -20.00612389586593309 ) ) ;
#8092 = ORIENTED_EDGE ( 'NONE', *, *, #11424, .F. ) ;
#8093 = EDGE_CURVE ( 'NONE', #1574, #3208, #4110, .T. ) ;
#8094 = CARTESIAN_POINT ( 'NONE',  ( 170.0000000000011369, 30.00000000000008882, 25.00000000000000000 ) ) ;
#8095 = CARTESIAN_POINT ( 'NONE',  ( 25.00000000000000355, 445.0000000000000568, -105.0000000000000000 ) ) ;
#8096 = VERTEX_POINT ( 'NONE', #50 ) ;
#8097 = PLANE ( 'NONE',  #11385 ) ;
#8098 = CARTESIAN_POINT ( 'NONE',  ( 24.99999999999999645, 345.0000000000000568, -95.00000000000000000 ) ) ;
#8099 = ORIENTED_EDGE ( 'NONE', *, *, #2233, .F. ) ;
#8100 = DIRECTION ( 'NONE',  ( -0.000000000000000000, -1.000000000000000000, -0.000000000000000000 ) ) ;
#8101 = CARTESIAN_POINT ( 'NONE',  ( 6.000000000000000888, 50.00000000000000000, 60.00000000000002132 ) ) ;
#8102 = CARTESIAN_POINT ( 'NONE',  ( 2.500000000000000000, 2.357898499370431722, -2.818925648462311528E-15 ) ) ;
#8103 = ORIENTED_EDGE ( 'NONE', *, *, #7421, .T. ) ;
#8104 = CYLINDRICAL_SURFACE ( 'NONE', #9345, 22.00000000000000355 ) ;
#8105 = CARTESIAN_POINT ( 'NONE',  ( 74.29751312657262474, 18.66988058564614761, 24.83155917518388733 ) ) ;
#8106 = VERTEX_POINT ( 'NONE', #2933 ) ;
#8107 = ORIENTED_EDGE ( 'NONE', *, *, #1750, .T. ) ;
#8108 = VECTOR ( 'NONE', #6853, 1000.000000000000114 ) ;
#8109 = CARTESIAN_POINT ( 'NONE',  ( 76.23711339313383917, 15.46430896355019158, 22.12715364262389883 ) ) ;
#8110 = CARTESIAN_POINT ( 'NONE',  ( 27.30107202361637775, 86.87046582918780757, 12.43589427268144831 ) ) ;
#8111 = ORIENTED_EDGE ( 'NONE', *, *, #11055, .F. ) ;
#8112 = FACE_OUTER_BOUND ( 'NONE', #6677, .T. ) ;
#8113 = CARTESIAN_POINT ( 'NONE',  ( 74.16198487146469631, 40.33897449742281083, 25.00000000000000000 ) ) ;
#8114 = ORIENTED_EDGE ( 'NONE', *, *, #1301, .T. ) ;
#8115 = EDGE_CURVE ( 'NONE', #5989, #12062, #11718, .T. ) ;
#8116 = CARTESIAN_POINT ( 'NONE',  ( -12.32411137850302119, 23.28349364905396612, 79.50000000000000000 ) ) ;
#8117 = EDGE_CURVE ( 'NONE', #7450, #1669, #9467, .T. ) ;
#8118 = LINE ( 'NONE', #275, #11084 ) ;
#8119 = CARTESIAN_POINT ( 'NONE',  ( -5.970153145843347347E-16, 114.6249999972688158, -3.250000000000000444 ) ) ;
#8120 = VECTOR ( 'NONE', #789, 1000.000000000000114 ) ;
#8121 = ORIENTED_EDGE ( 'NONE', *, *, #7138, .F. ) ;
#8122 = ORIENTED_EDGE ( 'NONE', *, *, #2585, .F. ) ;
#8123 = ORIENTED_EDGE ( 'NONE', *, *, #4213, .F. ) ;
#8124 = UNCERTAINTY_MEASURE_WITH_UNIT (LENGTH_MEASURE( 1.000000000000000082E-05 ), #7701, 'distance_accuracy_value', 'NONE');
#8125 = LINE ( 'NONE', #11947, #8227 ) ;
#8126 = DIRECTION ( 'NONE',  ( -0.4999999999999985012, 0.8660254037844394848, 0.000000000000000000 ) ) ;
#8127 = EDGE_CURVE ( 'NONE', #10877, #12351, #5698, .T. ) ;
#8128 = EDGE_CURVE ( 'NONE', #934, #3388, #6731, .T. ) ;
#8129 = LINE ( 'NONE', #6213, #58 ) ;
#8130 = FACE_OUTER_BOUND ( 'NONE', #10928, .T. ) ;
#8131 = CARTESIAN_POINT ( 'NONE',  ( -29.00531465893046601, 86.42397445338744433, -8.992822542244219619 ) ) ;
#8132 = DIRECTION ( 'NONE',  ( 7.011174048739587977E-15, 1.000000000000000000, 0.000000000000000000 ) ) ;
#8133 = CARTESIAN_POINT ( 'NONE',  ( 20.55500000000001748, 0.000000000000000000, 0.000000000000000000 ) ) ;
#8134 = CARTESIAN_POINT ( 'NONE',  ( -27.02024436599226576, 275.0000000000000000, -111.3324139431193345 ) ) ;
#8135 = CARTESIAN_POINT ( 'NONE',  ( 3.250000000000000444, 110.0000000000000000, 0.000000000000000000 ) ) ;
#8136 = CARTESIAN_POINT ( 'NONE',  ( 1.121994411437819084, 111.3749999986344079, -2.708734124999999437 ) ) ;
#8137 = PLANE ( 'NONE',  #3196 ) ;
#8138 = CIRCLE ( 'NONE', #11342, 100.0000000000000142 ) ;
#8139 = CIRCLE ( 'NONE', #11942, 73.00000000000002842 ) ;
#8140 = ADVANCED_FACE ( 'NONE', ( #2057 ), #7881, .T. ) ;
#8141 = EDGE_LOOP ( 'NONE', ( #11092, #12086, #4599 ) ) ;
#8142 = DIRECTION ( 'NONE',  ( 0.000000000000000000, 1.000000000000000000, 0.000000000000000000 ) ) ;
#8143 = ORIENTED_EDGE ( 'NONE', *, *, #11334, .T. ) ;
#8144 = DIRECTION ( 'NONE',  ( 1.000000000000000000, 0.000000000000000000, 0.000000000000000000 ) ) ;
#8145 = CARTESIAN_POINT ( 'NONE',  ( 74.16198487095665826, 20.00000000000009237, -25.00000000000000000 ) ) ;
#8146 = ORIENTED_EDGE ( 'NONE', *, *, #6299, .F. ) ;
#8147 = AXIS2_PLACEMENT_3D ( 'NONE', #9450, #4602, #1678 ) ;
#8148 = DIRECTION ( 'NONE',  ( -0.000000000000000000, -1.000000000000000000, -0.000000000000000000 ) ) ;
#8149 = CARTESIAN_POINT ( 'NONE',  ( 145.0000000000011369, 67.07106781186550393, 20.00000000000000000 ) ) ;
#8150 = ORIENTED_EDGE ( 'NONE', *, *, #7549, .F. ) ;
#8151 = CARTESIAN_POINT ( 'NONE',  ( -5.970153145843347347E-16, 113.7500000000000000, -3.250000000000000444 ) ) ;
#8152 = CIRCLE ( 'NONE', #10948, 14.99999999999999822 ) ;
#8153 = VERTEX_POINT ( 'NONE', #8587 ) ;
#8154 = CARTESIAN_POINT ( 'NONE',  ( -1.346194077712581150, 114.1874999972687874, 3.249999999999978240 ) ) ;
#8155 = ORIENTED_EDGE ( 'NONE', *, *, #10975, .F. ) ;
#8156 = ORIENTED_EDGE ( 'NONE', *, *, #3981, .T. ) ;
#8157 = CARTESIAN_POINT ( 'NONE',  ( -1.190781129305471087, 30.00000000000008882, 65.00000000000000000 ) ) ;
#8158 = CARTESIAN_POINT ( 'NONE',  ( -20.00000000000004263, 50.00000000000000000, 67.08203932499370126 ) ) ;
#8159 = ORIENTED_EDGE ( 'NONE', *, *, #9813, .F. ) ;
#8160 = CARTESIAN_POINT ( 'NONE',  ( 20.00000000000000000, 7.965803112215716020, 67.08203932499371547 ) ) ;
#8162 = CARTESIAN_POINT ( 'NONE',  ( -12.32411137850303184, 36.71650635094619730, 79.50000000000000000 ) ) ;
#8161 = VECTOR ( 'NONE', #3825, 1000.000000000000000 ) ;
#8163 = CARTESIAN_POINT ( 'NONE',  ( 20.00000000000000000, 54.99999999999999289, -67.08203932499371547 ) ) ;
#8164 = VECTOR ( 'NONE', #9948, 1000.000000000000114 ) ;
#8165 = ORIENTED_EDGE ( 'NONE', *, *, #1964, .F. ) ;
#8166 = CARTESIAN_POINT ( 'NONE',  ( 25.00000000000000000, 450.0000000000000568, -14.99999999999998934 ) ) ;
#8167 = AXIS2_PLACEMENT_3D ( 'NONE', #9493, #8688, #9618 ) ;
#8168 = ADVANCED_FACE ( 'NONE', ( #176, #9707 ), #1187, .T. ) ;
#8169 = EDGE_CURVE ( 'NONE', #12281, #9396, #6975, .T. ) ;
#8170 = CARTESIAN_POINT ( 'NONE',  ( 71.59624044336385396, 15.53386596841878919, 22.48149205125783823 ) ) ;
#8171 = EDGE_CURVE ( 'NONE', #4650, #10543, #2514, .T. ) ;
#8172 = CIRCLE ( 'NONE', #11177, 30.00000000000000000 ) ;
#8173 = ORIENTED_EDGE ( 'NONE', *, *, #11797, .F. ) ;
#8174 = FACE_OUTER_BOUND ( 'NONE', #9656, .T. ) ;
#8175 = CARTESIAN_POINT ( 'NONE',  ( 0.000000000000000000, 75.00000000000001421, 0.000000000000000000 ) ) ;
#8176 = ORIENTED_EDGE ( 'NONE', *, *, #9732, .F. ) ;
#8177 = FACE_BOUND ( 'NONE', #3492, .T. ) ;
#8178 = CARTESIAN_POINT ( 'NONE',  ( 71.43628325305886051, 49.01507604668937290, 22.85167202658856667 ) ) ;
#8179 = ORIENTED_EDGE ( 'NONE', *, *, #8210, .T. ) ;
#8180 = CARTESIAN_POINT ( 'NONE',  ( 0.000000000000000000, 115.0000000000000142, 0.000000000000000000 ) ) ;
#8181 = LINE ( 'NONE', #1649, #3323 ) ;
#8182 = CARTESIAN_POINT ( 'NONE',  ( 1.915364268218909594, 113.4374999986344079, 1.915364268218909594 ) ) ;
#8183 = VECTOR ( 'NONE', #1566, 1000.000000000000114 ) ;
#8184 = AXIS2_PLACEMENT_3D ( 'NONE', #825, #10219, #12112 ) ;
#8185 = B_SPLINE_CURVE_WITH_KNOTS ( 'NONE', 3,
 ( #5297, #11908, #2420, #5173 ),
 .UNSPECIFIED., .F., .F.,
 ( 4, 4 ),
 ( 0.0002502309401076743193, 0.0005002309401076760051 ),
 .UNSPECIFIED. ) ;
#8186 = ORIENTED_EDGE ( 'NONE', *, *, #5977, .T. ) ;
#8187 = LINE ( 'NONE', #1721, #10026 ) ;
#8188 = AXIS2_PLACEMENT_3D ( 'NONE', #795, #3906, #8439 ) ;
#8189 = CARTESIAN_POINT ( 'NONE',  ( -27.96741528345882344, 86.27927944434871677, -11.41192941739715927 ) ) ;
#8190 = LINE ( 'NONE', #11449, #11403 ) ;
#8191 = DIRECTION ( 'NONE',  ( 0.000000000000000000, 0.000000000000000000, -1.000000000000000000 ) ) ;
#8192 = CARTESIAN_POINT ( 'NONE',  ( -31.88521078284829713, 84.49999999999997158, -10.10362971081849004 ) ) ;
#8193 = CARTESIAN_POINT ( 'NONE',  ( 34.84121487603211875, 75.26794919243111792, -7.660254037844449471 ) ) ;
#8194 = CARTESIAN_POINT ( 'NONE',  ( 13.11583011321536141, 25.39745421660067848, 73.84506090661903954 ) ) ;
#8195 = CARTESIAN_POINT ( 'NONE',  ( -25.00000000000000000, 345.0000000000000568, -29.99999999999999289 ) ) ;
#8196 = CARTESIAN_POINT ( 'NONE',  ( -3.250000000000000444, 111.4375000000000000, 1.346194077712559389 ) ) ;
#8197 = CARTESIAN_POINT ( 'NONE',  ( 1.224646799147353059E-15, 110.0000000000000000, -9.999999999999998224 ) ) ;
#8198 = CIRCLE ( 'NONE', #4832, 72.00000000000002842 ) ;
#8199 = EDGE_CURVE ( 'NONE', #10214, #4695, #7786, .T. ) ;
#8200 = CARTESIAN_POINT ( 'NONE',  ( 0.000000000000000000, 110.0000000000000000, -15.00000000000000000 ) ) ;
#8201 = VERTEX_POINT ( 'NONE', #3114 ) ;
#8202 = CARTESIAN_POINT ( 'NONE',  ( 1.316495309083405051E-14, 340.0000000000000000, -105.0000000000000284 ) ) ;
#8203 = ORIENTED_EDGE ( 'NONE', *, *, #3107, .F. ) ;
#8204 = CARTESIAN_POINT ( 'NONE',  ( 165.0000000000011369, 225.0000000000000853, 20.00000000000000000 ) ) ;
#8205 = CARTESIAN_POINT ( 'NONE',  ( 2.298097038856278918, 113.7499999972688158, -2.298097038856279806 ) ) ;
#8206 = ORIENTED_EDGE ( 'NONE', *, *, #9808, .T. ) ;
#8207 = VECTOR ( 'NONE', #877, 1000.000000000000000 ) ;
#8208 = FACE_OUTER_BOUND ( 'NONE', #6317, .T. ) ;
#8209 = LINE ( 'NONE', #10269, #5580 ) ;
#8210 = EDGE_CURVE ( 'NONE', #3340, #5994, #6857, .T. ) ;
#8211 = ORIENTED_EDGE ( 'NONE', *, *, #6836, .T. ) ;
#8212 = ADVANCED_FACE ( 'NONE', ( #11663 ), #10463, .F. ) ;
#8213 = DIRECTION ( 'NONE',  ( 0.4999999999999877875, -0.8660254037844457020, 0.000000000000000000 ) ) ;
#8214 = AXIS2_PLACEMENT_3D ( 'NONE', #6346, #10135, #5419 ) ;
#8215 = ORIENTED_EDGE ( 'NONE', *, *, #10811, .F. ) ;
#8216 = CARTESIAN_POINT ( 'NONE',  ( 0.000000000000000000, 122.5000000000000000, 0.000000000000000000 ) ) ;
#8217 = LINE ( 'NONE', #11035, #868 ) ;
#8218 = ORIENTED_EDGE ( 'NONE', *, *, #11977, .F. ) ;
#8219 = PLANE ( 'NONE',  #3813 ) ;
#8220 = ADVANCED_FACE ( 'NONE', ( #11480 ), #1994, .T. ) ;
#8221 = DIRECTION ( 'NONE',  ( 3.469446951953613203E-16, 0.000000000000000000, 1.000000000000000000 ) ) ;
#8222 = ORIENTED_EDGE ( 'NONE', *, *, #9455, .T. ) ;
#8223 = SURFACE_STYLE_USAGE ( .BOTH. , #7367 ) ;
#8224 = CARTESIAN_POINT ( 'NONE',  ( -25.00000000000000000, 445.0000000000000568, -29.99999999999999289 ) ) ;
#8225 = CARTESIAN_POINT ( 'NONE',  ( 0.000000000000000000, -1.178949249685218748, -2.041999999999998039 ) ) ;
#8226 = LINE ( 'NONE', #6309, #6204 ) ;
#8227 = VECTOR ( 'NONE', #7694, 1000.000000000000000 ) ;
#8228 = AXIS2_PLACEMENT_3D ( 'NONE', #11168, #1811, #1694 ) ;
#8229 = ORIENTED_EDGE ( 'NONE', *, *, #2123, .F. ) ;
#8230 = PLANE ( 'NONE',  #6575 ) ;
#8231 = FACE_OUTER_BOUND ( 'NONE', #5860, .T. ) ;
#8232 = EDGE_LOOP ( 'NONE', ( #687, #756, #5127, #11163 ) ) ;
#8233 = DIRECTION ( 'NONE',  ( -0.000000000000000000, -1.000000000000000000, -0.000000000000000000 ) ) ;
#8234 = CARTESIAN_POINT ( 'NONE',  ( 0.000000000000000000, 260.0000000000000000, 0.000000000000000000 ) ) ;
#8235 = TOROIDAL_SURFACE ( 'NONE', #2870, 90.00000000000002842, 10.00000000000000000 ) ;
#8236 = VERTEX_POINT ( 'NONE', #7727 ) ;
#8237 = CIRCLE ( 'NONE', #4665, 8.000000000000000000 ) ;
#8238 = ADVANCED_FACE ( 'NONE', ( #6795 ), #10959, .T. ) ;
#8239 = DIRECTION ( 'NONE',  ( 0.8660254037844385966, -0.5000000000000000000, 0.000000000000000000 ) ) ;
#8240 = CARTESIAN_POINT ( 'NONE',  ( 0.000000000000000000, 115.0000000000000142, -15.00000000000000000 ) ) ;
#8241 = ORIENTED_EDGE ( 'NONE', *, *, #6773, .F. ) ;
#8242 = EDGE_CURVE ( 'NONE', #7898, #7852, #9013, .T. ) ;
#8243 = CARTESIAN_POINT ( 'NONE',  ( 2.571758278209431110E-16, 165.0000000000000000, -2.099999999999988987 ) ) ;
#8244 = ADVANCED_FACE ( 'NONE', ( #1489 ), #11070, .T. ) ;
#8245 = LINE ( 'NONE', #12190, #10481 ) ;
#8246 = CARTESIAN_POINT ( 'NONE',  ( 3.250000000000000444, 114.8749999972688158, 0.000000000000000000 ) ) ;
#8247 = CARTESIAN_POINT ( 'NONE',  ( 1.658621287961228320E-16, 112.8124999986344079, 2.708734124999999882 ) ) ;
#8248 = ORIENTED_EDGE ( 'NONE', *, *, #8808, .T. ) ;
#8249 = AXIS2_PLACEMENT_3D ( 'NONE', #360, #4228, #5233 ) ;
#8250 = EDGE_LOOP ( 'NONE', ( #1117, #8222, #453, #8014, #7504, #9866, #9995 ) ) ;
#8251 = DIRECTION ( 'NONE',  ( 0.000000000000000000, -0.000000000000000000, 1.000000000000000000 ) ) ;
#8252 = EDGE_CURVE ( 'NONE', #3388, #11037, #3730, .T. ) ;
#8253 = CARTESIAN_POINT ( 'NONE',  ( -29.09218482426048524, 85.72793236853334520, -10.45696826948038982 ) ) ;
#8254 = CARTESIAN_POINT ( 'NONE',  ( 0.000000000000000000, 87.00000000000000000, -30.00000000000000000 ) ) ;
#8255 = AXIS2_PLACEMENT_3D ( 'NONE', #1126, #113, #943 ) ;
#8256 = DIRECTION ( 'NONE',  ( 1.000000000000000000, 0.000000000000000000, 0.000000000000000000 ) ) ;
#8257 = TOROIDAL_SURFACE ( 'NONE', #4483, 12.99999999999999822, 2.000000000000000000 ) ;
#8258 = CARTESIAN_POINT ( 'NONE',  ( -27.33018067101282256, 86.99999999999998579, -12.37179148263487960 ) ) ;
#8259 = DIRECTION ( 'NONE',  ( 0.000000000000000000, -0.000000000000000000, 1.000000000000000000 ) ) ;
#8260 = DIRECTION ( 'NONE',  ( 0.000000000000000000, 0.000000000000000000, 1.000000000000000000 ) ) ;
#8261 = DIRECTION ( 'NONE',  ( 0.000000000000000000, 0.4999999999999990008, -0.8660254037844391517 ) ) ;
#8262 = CARTESIAN_POINT ( 'NONE',  ( 3.250000000000000444, 112.0000000000000000, 0.000000000000000000 ) ) ;
#8263 = VECTOR ( 'NONE', #5964, 1000.000000000000000 ) ;
#8264 = DIRECTION ( 'NONE',  ( 0.000000000000000000, 1.000000000000000000, 0.000000000000000000 ) ) ;
#8265 = DIRECTION ( 'NONE',  ( 0.000000000000000000, -0.4999999999999976685, 0.8660254037844399289 ) ) ;
#8266 = AXIS2_PLACEMENT_3D ( 'NONE', #6670, #1934, #2234 ) ;
#8267 = EDGE_LOOP ( 'NONE', ( #10161, #3684, #6623, #10654 ) ) ;
#8268 = CARTESIAN_POINT ( 'NONE',  ( -12.57202939415815202, 23.71770838516814450, 80.00000000000000000 ) ) ;
#8269 = DIRECTION ( 'NONE',  ( 0.000000000000000000, 0.000000000000000000, -1.000000000000000000 ) ) ;
#8270 = CARTESIAN_POINT ( 'NONE',  ( 69.65901248891714204, 17.35373687154389444, -27.79625982057084244 ) ) ;
#8271 = ORIENTED_EDGE ( 'NONE', *, *, #713, .F. ) ;
#8272 = EDGE_CURVE ( 'NONE', #6450, #8096, #550, .T. ) ;
#8273 = VECTOR ( 'NONE', #3376, 1000.000000000000000 ) ;
#8274 = DIRECTION ( 'NONE',  ( -0.4999999999999985567, 0.8660254037844394848, 0.000000000000000000 ) ) ;
#8275 = EDGE_CURVE ( 'NONE', #5974, #7236, #7284, .T. ) ;
#8276 = CARTESIAN_POINT ( 'NONE',  ( -7.907287480251413925, 18.86666975080236597, 79.50000000000000000 ) ) ;
#8277 = EDGE_LOOP ( 'NONE', ( #11129, #4800, #8760, #2148 ) ) ;
#8278 = LINE ( 'NONE', #3729, #6779 ) ;
#8279 = CIRCLE ( 'NONE', #2720, 3.250000000000000444 ) ;
#8280 = EDGE_LOOP ( 'NONE', ( #11510, #4994, #8903, #10671 ) ) ;
#8281 = LINE ( 'NONE', #11161, #4542 ) ;
#8282 = DIRECTION ( 'NONE',  ( -1.000000000000000000, 0.000000000000000000, 0.000000000000000000 ) ) ;
#8283 = VERTEX_POINT ( 'NONE', #7159 ) ;
#8284 = CYLINDRICAL_SURFACE ( 'NONE', #6797, 15.00000000000000000 ) ;
#8285 = CARTESIAN_POINT ( 'NONE',  ( -27.67899820261485999, 88.38261385519929547, -11.05501148229834030 ) ) ;
#8286 = ORIENTED_EDGE ( 'NONE', *, *, #11916, .F. ) ;
#8287 = EDGE_CURVE ( 'NONE', #10583, #5385, #8185, .T. ) ;
#8288 = DIRECTION ( 'NONE',  ( 0.000000000000000000, 0.000000000000000000, -1.000000000000000000 ) ) ;
#8289 = DIRECTION ( 'NONE',  ( 0.000000000000000000, 0.000000000000000000, 1.000000000000000000 ) ) ;
#8290 = FACE_OUTER_BOUND ( 'NONE', #3737, .T. ) ;
#8291 = ORIENTED_EDGE ( 'NONE', *, *, #10455, .F. ) ;
#8292 = CARTESIAN_POINT ( 'NONE',  ( 6.000000000000000888, 62.00000000000000000, 60.00000000000002132 ) ) ;
#8293 = EDGE_CURVE ( 'NONE', #11519, #7192, #5117, .T. ) ;
#8294 = FACE_OUTER_BOUND ( 'NONE', #8896, .T. ) ;
#8295 = AXIS2_PLACEMENT_3D ( 'NONE', #3505, #2563, #6370 ) ;
#8296 = VERTEX_POINT ( 'NONE', #7959 ) ;
#8297 = EDGE_CURVE ( 'NONE', #2436, #8994, #1909, .T. ) ;
#8298 = FACE_OUTER_BOUND ( 'NONE', #5274, .T. ) ;
#8299 = EDGE_CURVE ( 'NONE', #9853, #6660, #7035, .T. ) ;
#8300 = CARTESIAN_POINT ( 'NONE',  ( -16.19078112930547064, 29.48268919737577320, 73.23154106273422315 ) ) ;
#8301 = ORIENTED_EDGE ( 'NONE', *, *, #3213, .T. ) ;
#8302 = CARTESIAN_POINT ( 'NONE',  ( 0.000000000000000000, 50.00000000000000000, 0.000000000000000000 ) ) ;
#8303 = CARTESIAN_POINT ( 'NONE',  ( -26.76795759904968364, 61.76795759904965877, 64.77864552555394084 ) ) ;
#8304 = ORIENTED_EDGE ( 'NONE', *, *, #9714, .T. ) ;
#8305 = DIRECTION ( 'NONE',  ( 0.000000000000000000, 1.000000000000000000, 0.000000000000000000 ) ) ;
#8306 = DIRECTION ( 'NONE',  ( 0.000000000000000000, 1.000000000000000000, 0.000000000000000000 ) ) ;
#8307 = LINE ( 'NONE', #9482, #5796 ) ;
#8308 = CARTESIAN_POINT ( 'NONE',  ( -1.915364268218908927, 112.9374999986344079, 1.915364268218909150 ) ) ;
#8309 = ORIENTED_EDGE ( 'NONE', *, *, #6837, .T. ) ;
#8310 = EDGE_LOOP ( 'NONE', ( #7816, #238, #3311, #4386 ) ) ;
#8311 = FILL_AREA_STYLE_COLOUR ( '', #11744 ) ;
#8312 = PLANE ( 'NONE',  #5062 ) ;
#8313 = DIRECTION ( 'NONE',  ( 0.000000000000000000, 1.000000000000000000, 0.000000000000000000 ) ) ;
#8314 = CARTESIAN_POINT ( 'NONE',  ( -32.86043907464384972, 76.99999999999998579, 8.246007242324683517 ) ) ;
#8315 = DIRECTION ( 'NONE',  ( 1.000000000000000000, 0.000000000000000000, -0.000000000000000000 ) ) ;
#8316 = CARTESIAN_POINT ( 'NONE',  ( 0.000000000000000000, 285.0000000000000568, 100.0000000000000284 ) ) ;
#8317 = CARTESIAN_POINT ( 'NONE',  ( -12.80572322781401695, 39.54834576183792194, 73.90120587261097285 ) ) ;
#8318 = VECTOR ( 'NONE', #236, 999.9999999999997726 ) ;
#8319 = CARTESIAN_POINT ( 'NONE',  ( 2.500000000000000000, 0.000000000000000000, 0.000000000000000000 ) ) ;
#8320 = MECHANICAL_DESIGN_GEOMETRIC_PRESENTATION_REPRESENTATION (  '', ( #356 ), #6142 ) ;
#8321 = CARTESIAN_POINT ( 'NONE',  ( -1.346194077712560944, 113.6875000000000000, -3.249999999999999556 ) ) ;
#8322 = CARTESIAN_POINT ( 'NONE',  ( 9.184850993605150311E-15, 50.00000000000000000, 75.00000000000001421 ) ) ;
#8323 = EDGE_CURVE ( 'NONE', #10309, #9788, #11770, .T. ) ;
#8324 = ADVANCED_FACE ( 'NONE', ( #10835 ), #1365, .T. ) ;
#8325 = AXIS2_PLACEMENT_3D ( 'NONE', #12171, #9648, #2866 ) ;
#8326 = CARTESIAN_POINT ( 'NONE',  ( 1.346194077712572934, 112.6874999972688158, -3.249999999999987121 ) ) ;
#8327 = VERTEX_POINT ( 'NONE', #10322 ) ;
#8328 = CARTESIAN_POINT ( 'NONE',  ( 0.000000000000000000, -1.178949249685214307, 2.042000000000001592 ) ) ;
#8329 = DIRECTION ( 'NONE',  ( -1.000000000000000000, 0.000000000000000000, 0.000000000000000000 ) ) ;
#8330 = LINE ( 'NONE', #6594, #2905 ) ;
#8331 = ORIENTED_EDGE ( 'NONE', *, *, #5561, .F. ) ;
#8332 = CARTESIAN_POINT ( 'NONE',  ( 1.200153863164406345E-14, 265.0000000000000000, 98.00000000000001421 ) ) ;
#8333 = DIRECTION ( 'NONE',  ( 0.000000000000000000, 1.000000000000000000, 0.000000000000000000 ) ) ;
#8334 = ORIENTED_EDGE ( 'NONE', *, *, #3432, .F. ) ;
#8335 = CARTESIAN_POINT ( 'NONE',  ( 0.000000000000000000, 50.00000000000000000, 0.000000000000000000 ) ) ;
#8336 = ORIENTED_EDGE ( 'NONE', *, *, #638, .F. ) ;
#8337 = CARTESIAN_POINT ( 'NONE',  ( 0.000000000000000000, 115.0000000000000000, 0.000000000000000000 ) ) ;
#8338 = AXIS2_PLACEMENT_3D ( 'NONE', #2730, #1740, #5549 ) ;
#8340 = ORIENTED_EDGE ( 'NONE', *, *, #10307, .F. ) ;
#8339 = CARTESIAN_POINT ( 'NONE',  ( 2.020667218593133416E-14, 63.00000000000000000, 70.00000000000000000 ) ) ;
#8341 = ORIENTED_EDGE ( 'NONE', *, *, #11085, .F. ) ;
#8342 = CIRCLE ( 'NONE', #10538, 25.00000000000000000 ) ;
#8343 = CARTESIAN_POINT ( 'NONE',  ( 0.000000000000000000, 63.00000000000000000, 0.000000000000000000 ) ) ;
#8344 = DIRECTION ( 'NONE',  ( 0.000000000000000000, -0.8660254037844390407, -0.4999999999999993339 ) ) ;
#8345 = EDGE_LOOP ( 'NONE', ( #6072, #4123, #5577, #2711, #8864, #3274, #11231, #11727, #1867, #11599, #6996, #8304, #1179, #11251, #3120, #6578, #11615, #9961, #11384, #4673, #4865, #8744, #9719, #611, #3124, #7787, #17, #12099, #8686, #100, #6234, #11979, #162, #1625, #7604, #1699, #10784, #8143, #156, #8103, #1487, #11998, #10635, #8993, #6883, #10345, #67, #8420 ) ) ;
#8346 = DIRECTION ( 'NONE',  ( 0.000000000000000000, 0.000000000000000000, 1.000000000000000000 ) ) ;
#8347 = FACE_OUTER_BOUND ( 'NONE', #3295, .T. ) ;
#8348 = CARTESIAN_POINT ( 'NONE',  ( 0.000000000000000000, 77.00000000000000000, 0.000000000000000000 ) ) ;
#8349 = CARTESIAN_POINT ( 'NONE',  ( -9.726035167149728267, 35.21650635094616888, 79.50000000000000000 ) ) ;
#8350 = ORIENTED_EDGE ( 'NONE', *, *, #2614, .T. ) ;
#8351 = CARTESIAN_POINT ( 'NONE',  ( 1.121994411437819084, 111.3749999986344221, -2.708734124999999437 ) ) ;
#8352 = DIRECTION ( 'NONE',  ( 0.000000000000000000, -1.000000000000000000, 0.000000000000000000 ) ) ;
#8353 = VECTOR ( 'NONE', #1268, 1000.000000000000000 ) ;
#8354 = EDGE_CURVE ( 'NONE', #7290, #4162, #3908, .T. ) ;
#8355 = ORIENTED_EDGE ( 'NONE', *, *, #11393, .T. ) ;
#8356 = LINE ( 'NONE', #6506, #7940 ) ;
#8357 = CARTESIAN_POINT ( 'NONE',  ( -16.19078112930547064, 30.00000000000008882, 73.23154106273422315 ) ) ;
#8358 = ORIENTED_EDGE ( 'NONE', *, *, #11281, .T. ) ;
#8359 = CARTESIAN_POINT ( 'NONE',  ( 0.000000000000000000, 0.000000000000000000, 0.000000000000000000 ) ) ;
#8360 = CARTESIAN_POINT ( 'NONE',  ( 1.408343819019456413E-14, 290.0000000000000568, 115.0000000000000284 ) ) ;
#8361 = ORIENTED_EDGE ( 'NONE', *, *, #7250, .F. ) ;
#8362 = CIRCLE ( 'NONE', #2395, 105.0000000000000568 ) ;
#8363 = VECTOR ( 'NONE', #2270, 1000.000000000000000 ) ;
#8364 = CARTESIAN_POINT ( 'NONE',  ( 0.000000000000000000, 275.0000000000000000, 0.000000000000000000 ) ) ;
#8365 = CARTESIAN_POINT ( 'NONE',  ( 5.525725221640833240, 18.86666975080242992, 79.50000000000000000 ) ) ;
#8366 = CARTESIAN_POINT ( 'NONE',  ( 1.915364268218909150, 113.6874999986344079, 1.915364268218909150 ) ) ;
#8367 = EDGE_CURVE ( 'NONE', #6640, #11813, #12073, .T. ) ;
#8368 = CARTESIAN_POINT ( 'NONE',  ( -18.80690714323172941, 275.0000000000000000, -123.5771024247852665 ) ) ;
#8369 = EDGE_CURVE ( 'NONE', #10487, #3643, #4036, .T. ) ;
#8370 = EDGE_LOOP ( 'NONE', ( #235, #3605, #7240, #6049 ) ) ;
#8371 = AXIS2_PLACEMENT_3D ( 'NONE', #5718, #4770, #1037 ) ;
#8372 = VECTOR ( 'NONE', #1818, 1000.000000000000000 ) ;
#8373 = DIRECTION ( 'NONE',  ( 0.5000000000000066613, 0.8660254037844347108, 0.000000000000000000 ) ) ;
#8374 = CARTESIAN_POINT ( 'NONE',  ( 170.0000000000011369, 35.00000000000004974, -19.99999999999999645 ) ) ;
#8375 = AXIS2_PLACEMENT_3D ( 'NONE', #10788, #11554, #5131 ) ;
#8376 = CARTESIAN_POINT ( 'NONE',  ( 0.000000000000000000, 20.00000000000009237, 25.00000000000000000 ) ) ;
#8377 = PLANE ( 'NONE',  #4969 ) ;
#8378 = CARTESIAN_POINT ( 'NONE',  ( 7.344472908539098732, 24.78349364905406205, 79.50000000000000000 ) ) ;
#8379 = ADVANCED_FACE ( 'NONE', ( #10390 ), #10261, .F. ) ;
#8380 = CIRCLE ( 'NONE', #2415, 75.00000000000002842 ) ;
#8381 = DIRECTION ( 'NONE',  ( 0.000000000000000000, 1.000000000000000000, 0.000000000000000000 ) ) ;
#8382 = LINE ( 'NONE', #4648, #10382 ) ;
#8383 = CARTESIAN_POINT ( 'NONE',  ( -3.250000000000001776, 110.5625000000000000, -1.346194077712558723 ) ) ;
#8384 = CARTESIAN_POINT ( 'NONE',  ( 10.19254911989241386, 23.71650635094626836, 80.00000000000000000 ) ) ;
#8385 = AXIS2_PLACEMENT_3D ( 'NONE', #12013, #11268, #599 ) ;
#8386 = CIRCLE ( 'NONE', #9983, 25.00000000000000000 ) ;
#8387 = CARTESIAN_POINT ( 'NONE',  ( 20.00000000000000355, 63.00000000000000000, 57.08203932499370836 ) ) ;
#8388 = ORIENTED_EDGE ( 'NONE', *, *, #10326, .F. ) ;
#8389 = CARTESIAN_POINT ( 'NONE',  ( 0.000000000000000000, 52.00000000000000711, -72.00000000000002842 ) ) ;
#8390 = ADVANCED_FACE ( 'NONE', ( #6655 ), #3702, .T. ) ;
#8391 = LINE ( 'NONE', #12213, #10445 ) ;
#8392 = EDGE_CURVE ( 'NONE', #2119, #3216, #4475, .T. ) ;
#8393 = LINE ( 'NONE', #12335, #6093 ) ;
#8394 = ORIENTED_EDGE ( 'NONE', *, *, #196, .F. ) ;
#8395 = CARTESIAN_POINT ( 'NONE',  ( -27.02024436599226576, 285.0000000000000568, -111.3324139431193345 ) ) ;
#8396 = CARTESIAN_POINT ( 'NONE',  ( 0.000000000000000000, 340.0000000000000000, 0.000000000000000000 ) ) ;
#8397 = EDGE_CURVE ( 'NONE', #4162, #3178, #8330, .T. ) ;
#8398 = VERTEX_POINT ( 'NONE', #11215 ) ;
#8399 = LINE ( 'NONE', #7595, #4772 ) ;
#8400 =( BOUNDED_SURFACE ( )  B_SPLINE_SURFACE ( 1, 2, ( 
 ( #10857, #2377, #3382, #6186, #10983, #2447, #10040, #12177, #3685, #7612, #10480, #2748, #5508, #8351, #2629, #4741, #8532, #9528, #4558, #8414, #11421, #12298, #6556, #10346, #3627, #1168, #9404, #6436, #1817, #10224, #7435, #6678, #951, #2872, #10290, #887, #1942, #1700, #3811, #5750, #4681, #1010, #5628, #7372, #11239, #5566, #8473, #4620, #6502, #2687, #7551, #3745, #1758, #4809, #12114, #11361, #9343, #2812, #6616, #11174, #9287, #10411, #1874, #769, #829 ),
 ( #3566, #12239, #7493, #11304, #5688, #9471, #8596, #246, #6740, #2241, #5059, #7671, #308, #6865, #4058, #1252, #1194, #10719, #10534, #10660, #5871, #2179, #1314, #6050, #9653, #9778, #2127, #3121, #2998, #7849, #6803, #11669, #5929, #9712, #6924, #3996, #8839, #4873, #57, #8782, #2001, #5990, #4118, #9836, #4935, #4995, #1068, #3937, #7907, #3179, #11726, #7735, #8660, #122, #6980, #183, #10783, #5809, #1133, #11488, #9595, #2940, #3873, #11547, #10599 ) ),
 .UNSPECIFIED., .F., .F., .F. ) 
 B_SPLINE_SURFACE_WITH_KNOTS ( ( 2, 2 ),
 ( 3, 2, 2, 2, 2, 2, 2, 2, 2, 2, 2, 2, 2, 2, 2, 2, 2, 2, 2, 2, 2, 2, 2, 2, 2, 2, 2, 2, 2, 2, 2, 2, 3 ),
 ( 0.000000000000000000, 1.000000000000000000 ),
 ( 0.000000000000000000, 0.03125000000000000000, 0.06250000000000000000, 0.09375000000000000000, 0.1250000000000000000, 0.1562500000000000000, 0.1875000000000000000, 0.2187500000000000000, 0.2500000000000000000, 0.2812500000000000000, 0.3125000000000000000, 0.3437500000000000000, 0.3750000000000000000, 0.4062500000000000000, 0.4375000000000000000, 0.4687500000000000000, 0.5000000000000000000, 0.5312500000000000000, 0.5625000000000000000, 0.5937500000000000000, 0.6250000000000000000, 0.6562500000000000000, 0.6875000000000000000, 0.7187500000000000000, 0.7500000000000000000, 0.7812500000000000000, 0.8125000000000000000, 0.8437500000000000000, 0.8750000000000000000, 0.9062500000000000000, 0.9375000000000000000, 0.9687500000000000000, 1.000000000000000000 ),
 .UNSPECIFIED. ) 
 GEOMETRIC_REPRESENTATION_ITEM ( )  RATIONAL_B_SPLINE_SURFACE ( (
 ( 1.000000000000000000, 0.9238795325112867385, 1.000000000000000000, 0.9238795325112867385, 1.000000000000000000, 0.9238795325112867385, 1.000000000000000000, 0.9238795325112867385, 1.000000000000000000, 0.9238795325112867385, 1.000000000000000000, 0.9238795325112867385, 1.000000000000000000, 0.9238795325112867385, 1.000000000000000000, 0.9238795325112867385, 1.000000000000000000, 0.9238795325112867385, 1.000000000000000000, 0.9238795325112867385, 1.000000000000000000, 0.9238795325112867385, 1.000000000000000000, 0.9238795325112867385, 1.000000000000000000, 0.9238795325112867385, 1.000000000000000000, 0.9238795325112867385, 1.000000000000000000, 0.9238795325112867385, 1.000000000000000000, 0.9238795325112867385, 1.000000000000000000, 0.9238795325112867385, 1.000000000000000000, 0.9238795325112867385, 1.000000000000000000, 0.9238795325112867385, 1.000000000000000000, 0.9238795325112867385, 1.000000000000000000, 0.9238795325112867385, 1.000000000000000000, 0.9238795325112867385, 1.000000000000000000, 0.9238795325112867385, 1.000000000000000000, 0.9238795325112867385, 1.000000000000000000, 0.9238795325112867385, 1.000000000000000000, 0.9238795325112867385, 1.000000000000000000, 0.9238795325112867385, 1.000000000000000000, 0.9238795325112867385, 1.000000000000000000, 0.9238795325112867385, 1.000000000000000000, 0.9238795325112867385, 1.000000000000000000, 0.9238795325112867385, 1.000000000000000000, 0.9238795325112867385, 1.000000000000000000),
 ( 1.000000000000000000, 0.9238795325112867385, 1.000000000000000000, 0.9238795325112867385, 1.000000000000000000, 0.9238795325112867385, 1.000000000000000000, 0.9238795325112867385, 1.000000000000000000, 0.9238795325112867385, 1.000000000000000000, 0.9238795325112867385, 1.000000000000000000, 0.9238795325112867385, 1.000000000000000000, 0.9238795325112867385, 1.000000000000000000, 0.9238795325112867385, 1.000000000000000000, 0.9238795325112867385, 1.000000000000000000, 0.9238795325112867385, 1.000000000000000000, 0.9238795325112867385, 1.000000000000000000, 0.9238795325112867385, 1.000000000000000000, 0.9238795325112867385, 1.000000000000000000, 0.9238795325112867385, 1.000000000000000000, 0.9238795325112867385, 1.000000000000000000, 0.9238795325112867385, 1.000000000000000000, 0.9238795325112867385, 1.000000000000000000, 0.9238795325112867385, 1.000000000000000000, 0.9238795325112867385, 1.000000000000000000, 0.9238795325112867385, 1.000000000000000000, 0.9238795325112867385, 1.000000000000000000, 0.9238795325112867385, 1.000000000000000000, 0.9238795325112867385, 1.000000000000000000, 0.9238795325112867385, 1.000000000000000000, 0.9238795325112867385, 1.000000000000000000, 0.9238795325112867385, 1.000000000000000000, 0.9238795325112867385, 1.000000000000000000, 0.9238795325112867385, 1.000000000000000000, 0.9238795325112867385, 1.000000000000000000, 0.9238795325112867385, 1.000000000000000000, 0.9238795325112867385, 1.000000000000000000) ) ) 
 REPRESENTATION_ITEM ( '' )  SURFACE ( )  );
#8401 = ORIENTED_EDGE ( 'NONE', *, *, #19, .T. ) ;
#8402 = CIRCLE ( 'NONE', #3042, 30.00000000000000000 ) ;
#8403 = LINE ( 'NONE', #6359, #7337 ) ;
#8405 = VERTEX_POINT ( 'NONE', #3724 ) ;
#8404 = CARTESIAN_POINT ( 'NONE',  ( 0.000000000000000000, 340.0000000000000000, -115.0000000000000284 ) ) ;
#8406 = ORIENTED_EDGE ( 'NONE', *, *, #8682, .T. ) ;
#8407 = DIRECTION ( 'NONE',  ( 0.000000000000000000, 1.000000000000000000, 0.000000000000000000 ) ) ;
#8408 = ORIENTED_EDGE ( 'NONE', *, *, #11109, .F. ) ;
#8409 =( LENGTH_UNIT ( ) NAMED_UNIT ( * ) SI_UNIT ( .MILLI., .METRE. ) );
#8410 = CARTESIAN_POINT ( 'NONE',  ( -20.00000000000000355, 7.965803112215716020, -57.08203932499370836 ) ) ;
#8411 = CARTESIAN_POINT ( 'NONE',  ( 7.594472908539098732, 25.21650635094628257, 79.50000000000000000 ) ) ;
#8412 = CARTESIAN_POINT ( 'NONE',  ( 145.0000000000011369, 230.0000000000000853, -20.00000000000000000 ) ) ;
#8413 = ORIENTED_EDGE ( 'NONE', *, *, #5597, .T. ) ;
#8414 = CARTESIAN_POINT ( 'NONE',  ( 1.121994411437818862, 111.7499999986344079, 2.708734124999999882 ) ) ;
#8415 = VECTOR ( 'NONE', #10149, 1000.000000000000000 ) ;
#8416 = DIRECTION ( 'NONE',  ( 0.000000000000000000, -0.8660254037844401509, -0.4999999999999974465 ) ) ;
#8417 = ORIENTED_EDGE ( 'NONE', *, *, #6076, .F. ) ;
#8418 = CARTESIAN_POINT ( 'NONE',  ( 0.000000000000000000, 110.0000000000000000, 9.999999999999998224 ) ) ;
#8419 = DIRECTION ( 'NONE',  ( 0.000000000000000000, 0.000000000000000000, 1.000000000000000000 ) ) ;
#8420 = ORIENTED_EDGE ( 'NONE', *, *, #8449, .T. ) ;
#8421 = CARTESIAN_POINT ( 'NONE',  ( 32.05000697088088657, 85.26794919243110371, 9.660254037844429931 ) ) ;
#8422 = FACE_BOUND ( 'NONE', #6871, .T. ) ;
#8423 = VECTOR ( 'NONE', #5038, 1000.000000000000000 ) ;
#8424 = ORIENTED_EDGE ( 'NONE', *, *, #2844, .F. ) ;
#8425 = DIRECTION ( 'NONE',  ( 0.000000000000000000, -1.000000000000000000, 0.000000000000000000 ) ) ;
#8426 = DIRECTION ( 'NONE',  ( -0.000000000000000000, -1.000000000000000000, -0.000000000000000000 ) ) ;
#8427 = EDGE_CURVE ( 'NONE', #6026, #5348, #8393, .T. ) ;
#8428 = CARTESIAN_POINT ( 'NONE',  ( -2.708734124999999882, 114.0624999986344079, 3.317242575922456639E-16 ) ) ;
#8429 = ADVANCED_FACE ( 'NONE', ( #12153 ), #5481, .F. ) ;
#8430 = DIRECTION ( 'NONE',  ( 0.000000000000000000, 1.000000000000000000, 0.000000000000000000 ) ) ;
#8431 = ORIENTED_EDGE ( 'NONE', *, *, #8074, .T. ) ;
#8432 = VECTOR ( 'NONE', #6073, 1000.000000000000000 ) ;
#8433 = AXIS2_PLACEMENT_3D ( 'NONE', #7037, #7226, #9832 ) ;
#8434 = DIRECTION ( 'NONE',  ( 0.000000000000000000, 0.000000000000000000, 1.000000000000000000 ) ) ;
#8435 = ORIENTED_EDGE ( 'NONE', *, *, #2291, .F. ) ;
#8436 = CARTESIAN_POINT ( 'NONE',  ( -33.64113847583112715, 77.00000000000000000, 8.529771698700599813 ) ) ;
#8437 = CARTESIAN_POINT ( 'NONE',  ( -7.474274778359196070, 18.61666975080236597, 79.50000000000000000 ) ) ;
#8438 = CARTESIAN_POINT ( 'NONE',  ( -5.124469781714441119, 44.48424997675835613, 74.82642711344708175 ) ) ;
#8439 = DIRECTION ( 'NONE',  ( 1.000000000000000000, 0.000000000000000000, 0.000000000000000000 ) ) ;
#8440 = ADVANCED_FACE ( 'NONE', ( #1737 ), #3218, .F. ) ;
#8441 = ORIENTED_EDGE ( 'NONE', *, *, #5719, .F. ) ;
#8442 = AXIS2_PLACEMENT_3D ( 'NONE', #363, #6231, #8955 ) ;
#8443 = FACE_OUTER_BOUND ( 'NONE', #2643, .T. ) ;
#8444 = CIRCLE ( 'NONE', #8249, 2.099999999999988987 ) ;
#8445 = CARTESIAN_POINT ( 'NONE',  ( 0.000000000000000000, 2.357898499370431722, -2.818925648462311528E-15 ) ) ;
#8446 = AXIS2_PLACEMENT_3D ( 'NONE', #314, #4941, #10725 ) ;
#8447 = ORIENTED_EDGE ( 'NONE', *, *, #10707, .T. ) ;
#8448 = ADVANCED_FACE ( 'NONE', ( #1920 ), #3098, .T. ) ;
#8449 = EDGE_CURVE ( 'NONE', #11423, #1941, #2917, .T. ) ;
#8450 = CARTESIAN_POINT ( 'NONE',  ( 1.224646799147353059E-15, 165.0000000000000000, 9.999999999999998224 ) ) ;
#8451 = CARTESIAN_POINT ( 'NONE',  ( 0.000000000000000000, 75.00000000000001421, 0.000000000000000000 ) ) ;
#8452 = DIRECTION ( 'NONE',  ( -1.000000000000000000, 0.000000000000000000, -0.000000000000000000 ) ) ;
#8453 = ORIENTED_EDGE ( 'NONE', *, *, #1611, .F. ) ;
#8454 = DIRECTION ( 'NONE',  ( 1.000000000000000000, -0.000000000000000000, 1.224646799147353207E-16 ) ) ;
#8455 = PRODUCT ( 'Pulse _ Speed Control Dial', 'Pulse _ Speed Control Dial', '', ( #11482 ) ) ;
#8456 = DIRECTION ( 'NONE',  ( -0.000000000000000000, -0.000000000000000000, 1.000000000000000000 ) ) ;
#8457 = VECTOR ( 'NONE', #2851, 1000.000000000000000 ) ;
#8458 = ORIENTED_EDGE ( 'NONE', *, *, #11354, .T. ) ;
#8459 = DIRECTION ( 'NONE',  ( 0.000000000000000000, 0.000000000000000000, 1.000000000000000000 ) ) ;
#8460 = ADVANCED_FACE ( 'NONE', ( #99 ), #9632, .T. ) ;
#8461 = EDGE_LOOP ( 'NONE', ( #5019, #2686, #2801, #690 ) ) ;
#8462 = PLANE ( 'NONE',  #3551 ) ;
#8463 = DIRECTION ( 'NONE',  ( 0.000000000000000000, 1.000000000000000000, 0.000000000000000000 ) ) ;
#8464 = ORIENTED_EDGE ( 'NONE', *, *, #12103, .F. ) ;
#8465 = AXIS2_PLACEMENT_3D ( 'NONE', #1323, #2248, #11923 ) ;
#8466 = CARTESIAN_POINT ( 'NONE',  ( 140.0000000000011369, 67.07106781186550393, -20.00000000000000000 ) ) ;
#8467 = ORIENTED_EDGE ( 'NONE', *, *, #639, .T. ) ;
#8468 = CARTESIAN_POINT ( 'NONE',  ( -24.99999999999999289, 445.0000000000000568, -14.99999999999999289 ) ) ;
#8469 = DIRECTION ( 'NONE',  ( 0.000000000000000000, 1.000000000000000000, 0.000000000000000000 ) ) ;
#8470 = FACE_OUTER_BOUND ( 'NONE', #7486, .T. ) ;
#8471 =( BOUNDED_CURVE ( )  B_SPLINE_CURVE ( 2, ( #12018, #6340, #1603, #5410, #12085, #7339, #10800, #4375, #2260 ),
 .UNSPECIFIED., .F., .F. ) 
 B_SPLINE_CURVE_WITH_KNOTS ( ( 3, 2, 2, 2, 3 ),
 ( 0.1875000000000001665, 0.2187500000000001943, 0.2500000000000002220, 0.2812500000000002220, 0.3125000000000002776 ),
 .UNSPECIFIED. ) 
 CURVE ( )  GEOMETRIC_REPRESENTATION_ITEM ( )  RATIONAL_B_SPLINE_CURVE ( ( 0.9999999999999995559, 0.9238795325112871826, 1.000000000000000000, 0.9238795325112867385, 1.000000000000000000, 0.9238795325112867385, 1.000000000000000000, 0.9238795325112860723, 1.000000000000000666 ) ) 
 REPRESENTATION_ITEM ( '' )  );
#8472 = EDGE_LOOP ( 'NONE', ( #2557, #2528, #9957, #12273 ) ) ;
#8473 = CARTESIAN_POINT ( 'NONE',  ( 1.915364268218908705, 113.4374999986344079, -1.915364268218909594 ) ) ;
#8474 = CARTESIAN_POINT ( 'NONE',  ( 3.250000000000000444, 114.0000000000000000, 0.000000000000000000 ) ) ;
#8475 = EDGE_CURVE ( 'NONE', #3575, #7931, #602, .T. ) ;
#8476 = VECTOR ( 'NONE', #6150, 1000.000000000000000 ) ;
#8477 = VERTEX_POINT ( 'NONE', #2473 ) ;
#8478 = CARTESIAN_POINT ( 'NONE',  ( 0.000000000000000000, 340.0000000000000000, 0.000000000000000000 ) ) ;
#8479 = DIRECTION ( 'NONE',  ( 0.000000000000000000, 0.000000000000000000, 1.000000000000000000 ) ) ;
#8480 = EDGE_LOOP ( 'NONE', ( #7830, #7664, #6701, #4968 ) ) ;
#8481 = CARTESIAN_POINT ( 'NONE',  ( 1.990051048614449116E-16, 112.2500000000000000, 3.250000000000000444 ) ) ;
#8482 = CARTESIAN_POINT ( 'NONE',  ( 2.500000000000000000, -1.178949249685214307, 2.042000000000001592 ) ) ;
#8483 = ORIENTED_EDGE ( 'NONE', *, *, #8367, .F. ) ;
#8484 = CARTESIAN_POINT ( 'NONE',  ( -0.9407811293054709756, 43.00000000000008527, 79.50000000000000000 ) ) ;
#8485 = DIRECTION ( 'NONE',  ( 0.8660254037844377084, -0.5000000000000015543, 0.000000000000000000 ) ) ;
#8486 = CARTESIAN_POINT ( 'NONE',  ( -2.708734125000000326, 112.1249999986343937, -1.121994411437818195 ) ) ;
#8487 = VECTOR ( 'NONE', #652, 1000.000000000000000 ) ;
#8488 = DIRECTION ( 'NONE',  ( 0.7071067811865464625, 0.7071067811865486830, -2.453269466693394184E-16 ) ) ;
#8489 = ORIENTED_EDGE ( 'NONE', *, *, #8924, .F. ) ;
#8490 = FILL_AREA_STYLE ('',( #7692 ) ) ;
#8491 = EDGE_CURVE ( 'NONE', #931, #10229, #1799, .T. ) ;
#8492 = VERTEX_POINT ( 'NONE', #9940 ) ;
#8493 = EDGE_CURVE ( 'NONE', #7936, #5440, #3108, .T. ) ;
#8494 =( LENGTH_UNIT ( ) NAMED_UNIT ( * ) SI_UNIT ( .MILLI., .METRE. ) );
#8495 = ADVANCED_FACE ( 'NONE', ( #1477 ), #411, .F. ) ;
#8496 = CARTESIAN_POINT ( 'NONE',  ( 116.4243635975512490, 285.0000000000000568, 45.50129185973946733 ) ) ;
#8497 = ORIENTED_EDGE ( 'NONE', *, *, #865, .F. ) ;
#8498 = DIRECTION ( 'NONE',  ( 0.000000000000000000, 0.000000000000000000, -1.000000000000000000 ) ) ;
#8499 = CARTESIAN_POINT ( 'NONE',  ( 25.00000000000000000, 445.0000000000000568, -59.99999999999999289 ) ) ;
#8500 = CARTESIAN_POINT ( 'NONE',  ( 2.500000000000000000, 0.000000000000000000, 0.000000000000000000 ) ) ;
#8501 = CARTESIAN_POINT ( 'NONE',  ( 11.80921887069467324, 30.25000000000018474, 80.00000000000000000 ) ) ;
#8502 = ORIENTED_EDGE ( 'NONE', *, *, #5720, .T. ) ;
#8503 = FACE_OUTER_BOUND ( 'NONE', #6699, .T. ) ;
#8504 = UNCERTAINTY_MEASURE_WITH_UNIT (LENGTH_MEASURE( 1.000000000000000082E-05 ), #6756, 'distance_accuracy_value', 'NONE');
#8505 = EDGE_CURVE ( 'NONE', #3527, #6508, #9000, .T. ) ;
#8506 = EDGE_CURVE ( 'NONE', #7558, #3231, #6504, .T. ) ;
#8507 = CARTESIAN_POINT ( 'NONE',  ( 69.57792926911190534, 41.67137613650560013, -27.99850680361992517 ) ) ;
#8508 = DIRECTION ( 'NONE',  ( 0.5000000000000066613, 0.8660254037844347108, 0.000000000000000000 ) ) ;
#8509 = EDGE_LOOP ( 'NONE', ( #1738, #9705, #2986, #7718 ) ) ;
#8510 = CIRCLE ( 'NONE', #3150, 105.0000000000000426 ) ;
#8511 = DIRECTION ( 'NONE',  ( 0.000000000000000000, 0.000000000000000000, 1.000000000000000000 ) ) ;
#8512 = CARTESIAN_POINT ( 'NONE',  ( 0.000000000000000000, 345.0000000000000568, 0.000000000000000000 ) ) ;
#8513 = CARTESIAN_POINT ( 'NONE',  ( 74.38206444891756064, 18.35649441856873665, -24.72514820121006807 ) ) ;
#8514 = ORIENTED_EDGE ( 'NONE', *, *, #4544, .T. ) ;
#8515 = CARTESIAN_POINT ( 'NONE',  ( -12.57411137850301763, 23.71650635094618664, 79.50000000000000000 ) ) ;
#8516 = CARTESIAN_POINT ( 'NONE',  ( -1.440781129305282571, 17.00000000000009592, 79.50000000000000000 ) ) ;
#8517 = EDGE_LOOP ( 'NONE', ( #2228, #1878, #11052, #4934 ) ) ;
#8518 = CARTESIAN_POINT ( 'NONE',  ( 8.809218870694669690, 29.75000000000019540, 80.00000000000000000 ) ) ;
#8519 = VECTOR ( 'NONE', #12137, 1000.000000000000000 ) ;
#8520 = ADVANCED_FACE ( 'NONE', ( #4154 ), #4280, .F. ) ;
#8521 = ORIENTED_EDGE ( 'NONE', *, *, #7267, .T. ) ;
#8522 = CARTESIAN_POINT ( 'NONE',  ( -25.00000000000000000, 345.0000000000000568, -24.99999999999998934 ) ) ;
#8523 = PLANE ( 'NONE',  #7625 ) ;
#8524 = ORIENTED_EDGE ( 'NONE', *, *, #10893, .F. ) ;
#8525 = CARTESIAN_POINT ( 'NONE',  ( 31.92904760676809062, 76.99999999999998579, -7.658217335466646070 ) ) ;
#8526 = DIRECTION ( 'NONE',  ( -0.000000000000000000, 1.000000000000000000, -0.000000000000000000 ) ) ;
#8527 = VERTEX_POINT ( 'NONE', #347 ) ;
#8528 = CARTESIAN_POINT ( 'NONE',  ( -25.00000000000000000, 345.0000000000000568, -59.99999999999999289 ) ) ;
#8529 = CARTESIAN_POINT ( 'NONE',  ( 0.000000000000000000, 92.00000000000000000, 0.000000000000000000 ) ) ;
#8530 = DIRECTION ( 'NONE',  ( 0.000000000000000000, 0.000000000000000000, 1.000000000000000000 ) ) ;
#8531 = EDGE_LOOP ( 'NONE', ( #6931, #2500, #1749 ) ) ;
#8532 = CARTESIAN_POINT ( 'NONE',  ( 2.708734124999999882, 111.5624999986344079, 0.000000000000000000 ) ) ;
#8533 = CARTESIAN_POINT ( 'NONE',  ( 2.298097038856279806, 112.9999999972688158, 2.298097038856279806 ) ) ;
#8534 = AXIS2_PLACEMENT_3D ( 'NONE', #7941, #6958, #1227 ) ;
#8535 = VECTOR ( 'NONE', #3670, 1000.000000000000000 ) ;
#8536 = AXIS2_PLACEMENT_3D ( 'NONE', #7801, #4814, #3878 ) ;
#8537 = ORIENTED_EDGE ( 'NONE', *, *, #10811, .T. ) ;
#8538 = LINE ( 'NONE', #9717, #9127 ) ;
#8539 = DIRECTION ( 'NONE',  ( 0.000000000000000000, -0.000000000000000000, -1.000000000000000000 ) ) ;
#8540 = EDGE_LOOP ( 'NONE', ( #8877, #11338, #9996, #6291, #11040, #11518 ) ) ;
#8541 = CARTESIAN_POINT ( 'NONE',  ( -5.974274778359230709, 38.78525403784446723, 80.00000000000000000 ) ) ;
#8542 = CARTESIAN_POINT ( 'NONE',  ( 77.45966692414835109, 50.00000000000008527, 20.00000000000000000 ) ) ;
#8543 = ORIENTED_EDGE ( 'NONE', *, *, #926, .F. ) ;
#8544 = EDGE_CURVE ( 'NONE', #4065, #5525, #936, .T. ) ;
#8545 = EDGE_CURVE ( 'NONE', #4020, #2560, #7946, .T. ) ;
#8546 = DIRECTION ( 'NONE',  ( -1.000000000000000000, -0.000000000000000000, -0.000000000000000000 ) ) ;
#8547 = DIRECTION ( 'NONE',  ( 1.000000000000000000, 0.000000000000000000, 0.000000000000000000 ) ) ;
#8548 = VECTOR ( 'NONE', #812, 1000.000000000000000 ) ;
#8549 = DIRECTION ( 'NONE',  ( 1.000000000000000000, 0.000000000000000000, 0.000000000000000000 ) ) ;
#8550 = CIRCLE ( 'NONE', #9138, 100.0000000000000142 ) ;
#8551 = B_SPLINE_CURVE_WITH_KNOTS ( 'NONE', 3,
 ( #7091, #3351, #2345, #6152, #9820, #6033, #11650, #9942, #1418, #1234, #5041, #288, #10067, #3536, #11138, #9188, #3415, #604, #2537, #11955, #7212, #3473, #2597, #1543, #6403, #5346 ),
 .UNSPECIFIED., .F., .F.,
 ( 4, 2, 2, 2, 2, 2, 2, 2, 2, 2, 2, 2, 4 ),
 ( 1.055191096010040543E-17, 0.001946127227419493797, 0.002919190841129235166, 0.003892254454838976752, 0.005838381682258450382, 0.006811445295968177223, 0.007784508909677903196, 0.008757572523387630037, 0.009730636137097358612, 0.01167676336451680709, 0.01264982697822653740, 0.01362289059193626597, 0.01556901781935573700 ),
 .UNSPECIFIED. ) ;
#8552 = CARTESIAN_POINT ( 'NONE',  ( -1.915364268218908927, 111.9374999986344079, 1.915364268218909150 ) ) ;
#8553 = EDGE_CURVE ( 'NONE', #4222, #10014, #2343, .T. ) ;
#8554 = AXIS2_PLACEMENT_3D ( 'NONE', #3015, #7687, #8549 ) ;
#8555 = VERTEX_POINT ( 'NONE', #11774 ) ;
#8556 = AXIS2_PLACEMENT_3D ( 'NONE', #3476, #7464, #857 ) ;
#8557 = PRODUCT_DEFINITION_SHAPE ( 'NONE', 'NONE',  #11612 ) ;
#8558 = FACE_OUTER_BOUND ( 'NONE', #4764, .T. ) ;
#8559 = CARTESIAN_POINT ( 'NONE',  ( 0.000000000000000000, 115.0000000000000142, 0.000000000000000000 ) ) ;
#8560 = ORIENTED_EDGE ( 'NONE', *, *, #2658, .F. ) ;
#8561 = DIRECTION ( 'NONE',  ( 0.000000000000000000, 0.000000000000000000, 1.000000000000000000 ) ) ;
#8562 = CYLINDRICAL_SURFACE ( 'NONE', #4191, 70.00000000000001421 ) ;
#8563 = LINE ( 'NONE', #8501, #11392 ) ;
#8564 = AXIS2_PLACEMENT_3D ( 'NONE', #4085, #6081, #1221 ) ;
#8565 = PRESENTATION_LAYER_ASSIGNMENT (  '', '', ( #5399 ) ) ;
#8566 = B_SPLINE_CURVE_WITH_KNOTS ( 'NONE', 3,
 ( #6313, #771, #640, #2568 ),
 .UNSPECIFIED., .F., .F.,
 ( 4, 4 ),
 ( 0.000000000000000000, 0.001940928724149413795 ),
 .UNSPECIFIED. ) ;
#8567 = CARTESIAN_POINT ( 'NONE',  ( 74.29751312657262474, 41.33011941435380976, -24.83155917518393352 ) ) ;
#8568 = FILL_AREA_STYLE_COLOUR ( '', #10337 ) ;
#8569 = AXIS2_PLACEMENT_3D ( 'NONE', #3250, #7058, #10855 ) ;
#8570 = DIRECTION ( 'NONE',  ( -0.000000000000000000, 1.000000000000000000, -0.000000000000000000 ) ) ;
#8571 = PLANE ( 'NONE',  #2020 ) ;
#8572 = CARTESIAN_POINT ( 'NONE',  ( 18.80690714323171164, 285.0000000000000568, -123.5771024247852523 ) ) ;
#8573 = CARTESIAN_POINT ( 'NONE',  ( 72.28042146285945080, 14.83791805334885439, -20.04664579644849098 ) ) ;
#8574 = ORIENTED_EDGE ( 'NONE', *, *, #844, .F. ) ;
#8575 = CARTESIAN_POINT ( 'NONE',  ( -1.346194077712568049, 111.3124999999999858, 3.249999999999991118 ) ) ;
#8576 = CYLINDRICAL_SURFACE ( 'NONE', #10537, 70.00000000000001421 ) ;
#8577 = AXIS2_PLACEMENT_3D ( 'NONE', #10974, #9213, #11802 ) ;
#8578 = EDGE_CURVE ( 'NONE', #11226, #1340, #11953, .T. ) ;
#8579 = VERTEX_POINT ( 'NONE', #7209 ) ;
#8580 = DIRECTION ( 'NONE',  ( 1.224646799147352961E-16, 0.000000000000000000, -1.000000000000000000 ) ) ;
#8581 = AXIS2_PLACEMENT_3D ( 'NONE', #6402, #6217, #1478 ) ;
#8582 = ORIENTED_EDGE ( 'NONE', *, *, #9037, .F. ) ;
#8583 = CARTESIAN_POINT ( 'NONE',  ( -12.32411137850303184, 36.71650635094619730, 79.50000000000000000 ) ) ;
#8584 = CARTESIAN_POINT ( 'NONE',  ( 3.250000000000000444, 114.0000000000000000, 0.000000000000000000 ) ) ;
#8585 = VERTEX_POINT ( 'NONE', #11009 ) ;
#8586 = CARTESIAN_POINT ( 'NONE',  ( 30.55702146375036676, 77.00000000000001421, -5.949569453687718834 ) ) ;
#8587 = CARTESIAN_POINT ( 'NONE',  ( 0.000000000000000000, 50.00000000000000000, -75.00000000000001421 ) ) ;
#8588 = VERTEX_POINT ( 'NONE', #6275 ) ;
#8589 = EDGE_CURVE ( 'NONE', #11972, #1312, #10065, .T. ) ;
#8590 = CONTEXT_DEPENDENT_SHAPE_REPRESENTATION ( #7415, #5993 ) ;
#8591 = EDGE_CURVE ( 'NONE', #5183, #3340, #1624, .T. ) ;
#8592 = FACE_OUTER_BOUND ( 'NONE', #2990, .T. ) ;
#8593 = FACE_OUTER_BOUND ( 'NONE', #7658, .T. ) ;
#8594 = CARTESIAN_POINT ( 'NONE',  ( 0.000000000000000000, 265.0000000000000000, 100.0000000000000284 ) ) ;
#8595 = VERTEX_POINT ( 'NONE', #794 ) ;
#8596 = CARTESIAN_POINT ( 'NONE',  ( -1.915364268218909150, 110.6874999986344079, 1.915364268218909594 ) ) ;
#8597 = CARTESIAN_POINT ( 'NONE',  ( 145.0000000000011369, 230.0000000000000853, 20.00000000000000000 ) ) ;
#8598 = CIRCLE ( 'NONE', #5429, 9.999999999999994671 ) ;
#8599 = EDGE_CURVE ( 'NONE', #6043, #10619, #1130, .T. ) ;
#8600 = EDGE_CURVE ( 'NONE', #693, #4574, #1725, .T. ) ;
#8601 = ORIENTED_EDGE ( 'NONE', *, *, #6658, .T. ) ;
#8602 = LINE ( 'NONE', #5754, #7554 ) ;
#8603 = CARTESIAN_POINT ( 'NONE',  ( -8.008617612132468366, 16.62907246060994737, 74.57265862153481351 ) ) ;
#8604 = ORIENTED_EDGE ( 'NONE', *, *, #6032, .F. ) ;
#8605 = DIRECTION ( 'NONE',  ( 0.000000000000000000, -0.5000000000000013323, -0.8660254037844380415 ) ) ;
#8606 = CARTESIAN_POINT ( 'NONE',  ( 70.40708232491708429, 13.43343575954947156, 25.84664880093517070 ) ) ;
#8607 = ORIENTED_EDGE ( 'NONE', *, *, #8210, .F. ) ;
#8608 = ADVANCED_FACE ( 'NONE', ( #3653 ), #2312, .F. ) ;
#8609 = ADVANCED_FACE ( 'NONE', ( #9431 ), #7276, .T. ) ;
#8610 = DIRECTION ( 'NONE',  ( -1.000000000000000000, 0.000000000000000000, -0.000000000000000000 ) ) ;
#8611 = DIRECTION ( 'NONE',  ( 0.000000000000000000, 0.8660254037844407060, 0.4999999999999965028 ) ) ;
#8612 = CARTESIAN_POINT ( 'NONE',  ( -5.974274778359230709, 38.78525403784446723, 79.50000000000000000 ) ) ;
#8613 = CONICAL_SURFACE ( 'NONE', #9608, 2.055000000000000160, 0.7853981633974639331 ) ;
#8614 = DIRECTION ( 'NONE',  ( -0.000000000000000000, -1.000000000000000000, -0.000000000000000000 ) ) ;
#8615 = CARTESIAN_POINT ( 'NONE',  ( 2.298097038856278918, 110.8750000000000000, -2.298097038856279806 ) ) ;
#8616 = CARTESIAN_POINT ( 'NONE',  ( -1.121994411437819084, 113.8749999986344079, 2.708734124999999882 ) ) ;
#8617 = VERTEX_POINT ( 'NONE', #2716 ) ;
#8618 = VERTEX_POINT ( 'NONE', #2593 ) ;
#8619 = VECTOR ( 'NONE', #7347, 1000.000000000000114 ) ;
#8620 = EDGE_CURVE ( 'NONE', #10587, #7484, #1783, .T. ) ;
#8621 = FACE_OUTER_BOUND ( 'NONE', #1038, .T. ) ;
#8622 = PLANE ( 'NONE',  #10259 ) ;
#8623 = EDGE_LOOP ( 'NONE', ( #4927, #8215, #8640, #3613, #7510, #6633, #2724, #2201, #4368 ) ) ;
#8624 = DIRECTION ( 'NONE',  ( -0.000000000000000000, -1.000000000000000000, -0.000000000000000000 ) ) ;
#8625 = FACE_OUTER_BOUND ( 'NONE', #10598, .T. ) ;
#8626 = DIRECTION ( 'NONE',  ( 0.000000000000000000, 1.000000000000000000, 0.000000000000000000 ) ) ;
#8627 = FILL_AREA_STYLE_COLOUR ( '', #7580 ) ;
#8628 = ORIENTED_EDGE ( 'NONE', *, *, #11133, .F. ) ;
#8629 = ADVANCED_FACE ( 'NONE', ( #1842 ), #3591, .F. ) ;
#8630 = CARTESIAN_POINT ( 'NONE',  ( 74.70719529697929318, 42.54354230980619889, -24.30790125104183019 ) ) ;
#8631 = DIRECTION ( 'NONE',  ( 0.000000000000000000, 0.000000000000000000, 1.000000000000000000 ) ) ;
#8632 = CIRCLE ( 'NONE', #6464, 30.00000000000000000 ) ;
#8633 = CYLINDRICAL_SURFACE ( 'NONE', #419, 9.999999999999994671 ) ;
#8634 = CONICAL_SURFACE ( 'NONE', #4465, 75.00000000000001421, 0.7853981633974427279 ) ;
#8635 = DIRECTION ( 'NONE',  ( 0.000000000000000000, 0.000000000000000000, 1.000000000000000000 ) ) ;
#8636 = CARTESIAN_POINT ( 'NONE',  ( 71.99731494076550575, 14.95993129310641123, -21.09170898384848414 ) ) ;
#8637 = ORIENTED_EDGE ( 'NONE', *, *, #9434, .F. ) ;
#8638 = DIRECTION ( 'NONE',  ( -0.000000000000000000, -1.000000000000000000, -0.000000000000000000 ) ) ;
#8639 = CARTESIAN_POINT ( 'NONE',  ( 1.224646799147353533E-14, 285.0000000000000568, -100.0000000000000284 ) ) ;
#8640 = ORIENTED_EDGE ( 'NONE', *, *, #8754, .T. ) ;
#8641 = CARTESIAN_POINT ( 'NONE',  ( -25.00000000000000000, 445.0000000000000568, -59.99999999999999289 ) ) ;
#8642 = VECTOR ( 'NONE', #6535, 1000.000000000000000 ) ;
#8643 = CIRCLE ( 'NONE', #9639, 70.00000000000001421 ) ;
#8644 = ORIENTED_EDGE ( 'NONE', *, *, #11532, .T. ) ;
#8645 = EDGE_CURVE ( 'NONE', #7990, #10179, #11202, .T. ) ;
#8646 = DIRECTION ( 'NONE',  ( -0.7071067811865513475, -0.7071067811865437980, -0.000000000000000000 ) ) ;
#8647 = CARTESIAN_POINT ( 'NONE',  ( 21.00000000000000355, 0.000000000000000000, 0.000000000000000000 ) ) ;
#8648 = ORIENTED_EDGE ( 'NONE', *, *, #2766, .T. ) ;
#8649 = EDGE_CURVE ( 'NONE', #9737, #5931, #3711, .T. ) ;
#8650 = CARTESIAN_POINT ( 'NONE',  ( 1.734723475976807094E-14, 63.00000000000000000, 57.08203932499370836 ) ) ;
#8651 = DIRECTION ( 'NONE',  ( -0.8660254037844394848, 0.4999999999999985567, 0.000000000000000000 ) ) ;
#8652 = VERTEX_POINT ( 'NONE', #7517 ) ;
#8653 = APPLICATION_PROTOCOL_DEFINITION ( 'draft international standard', 'automotive_design', 1998, #5510 ) ;
#8654 = VECTOR ( 'NONE', #12082, 1000.000000000000114 ) ;
#8655 = LINE ( 'NONE', #4932, #10447 ) ;
#8656 = CIRCLE ( 'NONE', #10250, 12.99999999999999822 ) ;
#8657 = CARTESIAN_POINT ( 'NONE',  ( 0.000000000000000000, 0.000000000000000000, 0.000000000000000000 ) ) ;
#8658 = CARTESIAN_POINT ( 'NONE',  ( 5.525725221640833240, 18.86666975080242992, 80.00000000000000000 ) ) ;
#8659 = ORIENTED_EDGE ( 'NONE', *, *, #249, .F. ) ;
#8660 = CARTESIAN_POINT ( 'NONE',  ( 1.658621287961228566E-16, 113.5624999986344079, 2.708734125000000326 ) ) ;
#8661 = CARTESIAN_POINT ( 'NONE',  ( 3.249999999999999556, 111.8124999972688016, -1.346194077712561610 ) ) ;
#8662 = VECTOR ( 'NONE', #2011, 1000.000000000000000 ) ;
#8663 = ORIENTED_EDGE ( 'NONE', *, *, #4806, .F. ) ;
#8664 = EDGE_CURVE ( 'NONE', #12219, #5952, #733, .T. ) ;
#8665 = PLANE ( 'NONE',  #10738 ) ;
#8666 = CARTESIAN_POINT ( 'NONE',  ( 5.200000000000002842, 3.061616997868383634E-16, -2.500000000000000444 ) ) ;
#8667 = VERTEX_POINT ( 'NONE', #664 ) ;
#8668 = CARTESIAN_POINT ( 'NONE',  ( 140.0000000000011369, 225.0000000000000853, 20.00000000000000000 ) ) ;
#8669 = CARTESIAN_POINT ( 'NONE',  ( -97.61745645432043261, 285.0000000000000568, 78.07581056504542971 ) ) ;
#8670 = VERTEX_POINT ( 'NONE', #4460 ) ;
#8671 = CARTESIAN_POINT ( 'NONE',  ( 1.990051048614449116E-16, 110.2500000000000000, 3.250000000000000444 ) ) ;
#8672 = CARTESIAN_POINT ( 'NONE',  ( 0.000000000000000000, 50.00000000000000000, 0.000000000000000000 ) ) ;
#8673 = CARTESIAN_POINT ( 'NONE',  ( -5.970153145843347347E-16, 113.6249999972688158, -3.250000000000000444 ) ) ;
#8674 = APPLICATION_CONTEXT ( 'automotive_design' ) ;
#8675 = AXIS2_PLACEMENT_3D ( 'NONE', #630, #3736, #10152 ) ;
#8676 = LINE ( 'NONE', #4824, #9549 ) ;
#8677 = SPHERICAL_SURFACE ( 'NONE', #2788, 5.000000000000000000 ) ;
#8678 = CARTESIAN_POINT ( 'NONE',  ( 72.32495769890022075, 14.83846616281870467, 19.87825060515873687 ) ) ;
#8679 = ORIENTED_EDGE ( 'NONE', *, *, #8827, .F. ) ;
#8680 = SURFACE_SIDE_STYLE ('',( #7630 ) ) ;
#8681 = AXIS2_PLACEMENT_3D ( 'NONE', #11898, #10762, #10007 ) ;
#8682 = EDGE_CURVE ( 'NONE', #8789, #6619, #6901, .T. ) ;
#8683 = ORIENTED_EDGE ( 'NONE', *, *, #8127, .F. ) ;
#8684 = CARTESIAN_POINT ( 'NONE',  ( 0.000000000000000000, 216.0365690573663926, -15.00000000000000000 ) ) ;
#8685 = LINE ( 'NONE', #8867, #6892 ) ;
#8686 = ORIENTED_EDGE ( 'NONE', *, *, #1176, .F. ) ;
#8687 = CARTESIAN_POINT ( 'NONE',  ( 0.000000000000000000, 122.0000000000000000, 0.000000000000000000 ) ) ;
#8688 = DIRECTION ( 'NONE',  ( 0.000000000000000000, 1.000000000000000000, 0.000000000000000000 ) ) ;
#8689 = AXIS2_PLACEMENT_3D ( 'NONE', #4307, #5009, #2374 ) ;
#8690 = CARTESIAN_POINT ( 'NONE',  ( 170.0000000000011369, 225.0000000000000853, 25.00000000000000000 ) ) ;
#8691 = CARTESIAN_POINT ( 'NONE',  ( -4.975863863883684959E-16, 111.0624999986344079, -2.708734125000000326 ) ) ;
#8692 = EDGE_LOOP ( 'NONE', ( #2101, #2934, #12159 ) ) ;
#8693 = ORIENTED_EDGE ( 'NONE', *, *, #6038, .F. ) ;
#8694 = ORIENTED_EDGE ( 'NONE', *, *, #3864, .T. ) ;
#8695 = CARTESIAN_POINT ( 'NONE',  ( 71.74671581198448678, 44.73114732258832760, -21.97107035890099169 ) ) ;
#8696 = SURFACE_STYLE_USAGE ( .BOTH. , #1915 ) ;
#8697 = CARTESIAN_POINT ( 'NONE',  ( 29.09218482426055985, 85.72793236853330257, 10.45696826948034008 ) ) ;
#8698 = CARTESIAN_POINT ( 'NONE',  ( 18.80690714323171164, 275.0000000000000000, -123.5771024247852523 ) ) ;
#8699 = LINE ( 'NONE', #2106, #914 ) ;
#8700 = CARTESIAN_POINT ( 'NONE',  ( 75.14265900998621817, 16.66197922908980544, -23.72616954495079256 ) ) ;
#8701 = ORIENTED_EDGE ( 'NONE', *, *, #9975, .F. ) ;
#8702 = CARTESIAN_POINT ( 'NONE',  ( 0.000000000000000000, 45.00000000000008527, 0.000000000000000000 ) ) ;
#8703 = EDGE_CURVE ( 'NONE', #11813, #8705, #1662, .T. ) ;
#8704 = LINE ( 'NONE', #4786, #11141 ) ;
#8705 = VERTEX_POINT ( 'NONE', #6829 ) ;
#8706 = DIRECTION ( 'NONE',  ( 0.000000000000000000, 0.000000000000000000, -1.000000000000000000 ) ) ;
#8707 = EDGE_CURVE ( 'NONE', #6555, #7679, #4836, .T. ) ;
#8708 = VECTOR ( 'NONE', #6666, 1000.000000000000000 ) ;
#8709 = ORIENTED_EDGE ( 'NONE', *, *, #2470, .F. ) ;
#8710 = CARTESIAN_POINT ( 'NONE',  ( 0.000000000000000000, 65.00000000000000000, -75.00000000000002842 ) ) ;
#8711 = DIRECTION ( 'NONE',  ( 0.000000000000000000, 0.000000000000000000, -1.000000000000000000 ) ) ;
#8712 = VERTEX_POINT ( 'NONE', #6895 ) ;
#8713 = CARTESIAN_POINT ( 'NONE',  ( -3.250000000000001776, 111.4374999972688300, -1.346194077712558279 ) ) ;
#8714 = DIRECTION ( 'NONE',  ( -0.7236679289129653858, 0.000000000000000000, -0.6901483381584129218 ) ) ;
#8715 = VERTEX_POINT ( 'NONE', #12321 ) ;
#8716 = PRODUCT_CONTEXT ( 'NONE', #7643, 'mechanical' ) ;
#8717 = FACE_OUTER_BOUND ( 'NONE', #7721, .T. ) ;
#8718 = CARTESIAN_POINT ( 'NONE',  ( 0.000000000000000000, 115.0000000000000000, 0.000000000000000000 ) ) ;
#8719 = CIRCLE ( 'NONE', #3356, 105.0000000000000426 ) ;
#8720 = MANIFOLD_SOLID_BREP ( 'Cut-Extrude-Thin1', #7678 ) ;
#8721 = ORIENTED_EDGE ( 'NONE', *, *, #1152, .T. ) ;
#8722 = LINE ( 'NONE', #2362, #7564 ) ;
#8723 = CARTESIAN_POINT ( 'NONE',  ( 3.250000000000000444, 112.8749999972688158, 0.000000000000000000 ) ) ;
#8724 = EDGE_LOOP ( 'NONE', ( #760, #3288, #9295, #5870, #1305 ) ) ;
#8725 = CARTESIAN_POINT ( 'NONE',  ( -1.440781129305471087, 43.00000000000008527, 79.50000000000000000 ) ) ;
#8726 = DIRECTION ( 'NONE',  ( 0.000000000000000000, 0.000000000000000000, 1.000000000000000000 ) ) ;
#8727 = ORIENTED_EDGE ( 'NONE', *, *, #4771, .F. ) ;
#8728 = CARTESIAN_POINT ( 'NONE',  ( 25.00000000000000000, 445.0000000000000568, -14.99999999999998934 ) ) ;
#8729 = CARTESIAN_POINT ( 'NONE',  ( -12.32411137850303184, 36.71650635094619730, 79.50000000000000000 ) ) ;
#8730 = VERTEX_POINT ( 'NONE', #1098 ) ;
#8731 = CARTESIAN_POINT ( 'NONE',  ( -31.74999999999995737, 0.000000000000000000, 2.500000000000000444 ) ) ;
#8732 = LINE ( 'NONE', #10488, #7894 ) ;
#8733 = LINE ( 'NONE', #8612, #9154 ) ;
#8734 = CARTESIAN_POINT ( 'NONE',  ( 107.1104145097471445, 275.0000000000000000, 41.86118851096031079 ) ) ;
#8735 = CARTESIAN_POINT ( 'NONE',  ( -9.976035167149682081, 25.21650635094616533, 80.00000000000000000 ) ) ;
#8736 = EDGE_CURVE ( 'NONE', #11474, #3822, #10689, .T. ) ;
#8737 = CARTESIAN_POINT ( 'NONE',  ( 1.121994411437819084, 113.7499999986344221, 2.708734124999999882 ) ) ;
#8738 = CIRCLE ( 'NONE', #8167, 105.0000000000000426 ) ;
#8739 = VERTEX_POINT ( 'NONE', #5779 ) ;
#8740 = ORIENTED_EDGE ( 'NONE', *, *, #1177, .T. ) ;
#8741 = B_SPLINE_CURVE_WITH_KNOTS ( 'NONE', 3,
 ( #5252, #7978, #5942, #6003, #4128, #11806, #3194, #5076, #9790, #9913, #2317, #2194, #9977, #10675, #1383, #7919, #5192, #8972 ),
 .UNSPECIFIED., .F., .F.,
 ( 4, 2, 2, 2, 2, 2, 2, 2, 4 ),
 ( 0.000000000000000000, 0.001070780962355597030, 0.002141561924711194061, 0.003212342887066791091, 0.004283123849422388121, 0.005353904811777984718, 0.006424685774133582182, 0.007495466736489179646, 0.008566247698844776243 ),
 .UNSPECIFIED. ) ;
#8742 = DIRECTION ( 'NONE',  ( -0.000000000000000000, -1.000000000000000000, -0.000000000000000000 ) ) ;
#8743 = CARTESIAN_POINT ( 'NONE',  ( 0.000000000000000000, 127.0000000000000000, 0.000000000000000000 ) ) ;
#8744 = ORIENTED_EDGE ( 'NONE', *, *, #6347, .T. ) ;
#8745 = FACE_BOUND ( 'NONE', #1807, .T. ) ;
#8746 = VECTOR ( 'NONE', #750, 1000.000000000000000 ) ;
#8747 = CARTESIAN_POINT ( 'NONE',  ( 0.000000000000000000, 115.0000000000000000, 0.000000000000000000 ) ) ;
#8748 = DIRECTION ( 'NONE',  ( -1.000000000000000000, 0.000000000000000000, 0.000000000000000000 ) ) ;
#8749 = CARTESIAN_POINT ( 'NONE',  ( 27.96741528345890870, 86.27927944434865992, 11.41192941739706335 ) ) ;
#8750 = EDGE_CURVE ( 'NONE', #7578, #9737, #11638, .T. ) ;
#8751 = EDGE_CURVE ( 'NONE', #12189, #7290, #1036, .T. ) ;
#8752 = ORIENTED_EDGE ( 'NONE', *, *, #10125, .T. ) ;
#8753 = AXIS2_PLACEMENT_3D ( 'NONE', #12052, #10095, #9980 ) ;
#8754 = EDGE_CURVE ( 'NONE', #12288, #4547, #8016, .T. ) ;
#8755 = DIRECTION ( 'NONE',  ( 0.000000000000000000, 0.000000000000000000, 1.000000000000000000 ) ) ;
#8756 = CARTESIAN_POINT ( 'NONE',  ( 2.694222958124177204E-15, 92.00000000000000000, 22.00000000000000355 ) ) ;
#8757 = SURFACE_SIDE_STYLE ('',( #5103 ) ) ;
#8758 = CIRCLE ( 'NONE', #7965, 25.00000000000000000 ) ;
#8759 = CARTESIAN_POINT ( 'NONE',  ( 72.29800075079589305, 10.06258521785520976, -19.95946618966756958 ) ) ;
#8760 = ORIENTED_EDGE ( 'NONE', *, *, #6468, .F. ) ;
#8761 = CIRCLE ( 'NONE', #9951, 2.000000000000001776 ) ;
#8762 = LINE ( 'NONE', #1175, #10636 ) ;
#8763 = PRODUCT ( 'Central Drive Shaft Post', 'Central Drive Shaft Post', '', ( #1189 ) ) ;
#8764 = DIRECTION ( 'NONE',  ( 0.000000000000000000, 1.000000000000000000, 0.000000000000000000 ) ) ;
#8765 = ORIENTED_EDGE ( 'NONE', *, *, #1588, .T. ) ;
#8766 = FACE_OUTER_BOUND ( 'NONE', #281, .T. ) ;
#8767 = CIRCLE ( 'NONE', #11974, 2.700000000000000622 ) ;
#8768 = VECTOR ( 'NONE', #1955, 1000.000000000000000 ) ;
#8769 = EDGE_CURVE ( 'NONE', #12062, #2119, #3028, .T. ) ;
#8770 = ORIENTED_EDGE ( 'NONE', *, *, #5852, .F. ) ;
#8771 = EDGE_CURVE ( 'NONE', #2880, #1574, #3101, .T. ) ;
#8772 = DIRECTION ( 'NONE',  ( -0.000000000000000000, 1.000000000000000000, -0.000000000000000000 ) ) ;
#8773 = DIRECTION ( 'NONE',  ( -6.938893903907222067E-15, -1.000000000000000000, 0.000000000000000000 ) ) ;
#8774 = ORIENTED_EDGE ( 'NONE', *, *, #3560, .F. ) ;
#8775 = CARTESIAN_POINT ( 'NONE',  ( -0.9407811293054709756, 40.00000000000008527, 79.50000000000000000 ) ) ;
#8776 = ORIENTED_EDGE ( 'NONE', *, *, #3420, .F. ) ;
#8777 = AXIS2_PLACEMENT_3D ( 'NONE', #9908, #564, #5248 ) ;
#8778 = CARTESIAN_POINT ( 'NONE',  ( 4.025725221640669815, 38.53525403784453118, 79.50000000000000000 ) ) ;
#8779 = CIRCLE ( 'NONE', #3421, 5.000000000000000888 ) ;
#8780 = CARTESIAN_POINT ( 'NONE',  ( 13.80921887069452758, 30.00000000000009237, 65.00000000000000000 ) ) ;
#8781 = ORIENTED_EDGE ( 'NONE', *, *, #1137, .T. ) ;
#8782 = CARTESIAN_POINT ( 'NONE',  ( -2.708734125000000326, 112.7499999986343937, 1.121994411437818862 ) ) ;
#8783 = CARTESIAN_POINT ( 'NONE',  ( 1.346194077712559833, 113.6874999972688016, -3.250000000000000000 ) ) ;
#8784 = AXIS2_PLACEMENT_3D ( 'NONE', #10696, #7022, #10817 ) ;
#8785 = VECTOR ( 'NONE', #11899, 1000.000000000000000 ) ;
#8786 = ORIENTED_EDGE ( 'NONE', *, *, #10703, .T. ) ;
#8787 = LINE ( 'NONE', #7853, #2958 ) ;
#8788 = CYLINDRICAL_SURFACE ( 'NONE', #3280, 75.00000000000001421 ) ;
#8789 = VERTEX_POINT ( 'NONE', #2839 ) ;
#8790 = CARTESIAN_POINT ( 'NONE',  ( 165.0000000000011369, 225.0000000000000853, -20.00000000000000000 ) ) ;
#8791 = CARTESIAN_POINT ( 'NONE',  ( -7.474274778359198734, 41.38333024919781167, 80.00000000000000000 ) ) ;
#8792 = ORIENTED_EDGE ( 'NONE', *, *, #7138, .T. ) ;
#8793 = CARTESIAN_POINT ( 'NONE',  ( -2.298097038856279806, 110.6250000000000000, -2.298097038856279362 ) ) ;
#8794 = DIRECTION ( 'NONE',  ( 0.000000000000000000, 0.000000000000000000, -1.000000000000000000 ) ) ;
#8795 = DIRECTION ( 'NONE',  ( 0.000000000000000000, 0.000000000000000000, 1.000000000000000000 ) ) ;
#8796 = FACE_OUTER_BOUND ( 'NONE', #8849, .T. ) ;
#8797 = AXIS2_PLACEMENT_3D ( 'NONE', #5088, #10807, #4083 ) ;
#8798 = CARTESIAN_POINT ( 'NONE',  ( 2.708734124999999882, 112.6249999986343937, 1.121994411437819084 ) ) ;
#8799 = EDGE_LOOP ( 'NONE', ( #8291, #9537, #2137, #10084 ) ) ;
#8800 = ORIENTED_EDGE ( 'NONE', *, *, #1498, .F. ) ;
#8801 = LINE ( 'NONE', #11818, #885 ) ;
#8802 = FACE_OUTER_BOUND ( 'NONE', #11364, .T. ) ;
#8803 = CIRCLE ( 'NONE', #4042, 75.00000000000001421 ) ;
#8804 = ORIENTED_EDGE ( 'NONE', *, *, #8506, .T. ) ;
#8805 = EDGE_CURVE ( 'NONE', #8595, #7410, #4706, .T. ) ;
#8806 = CARTESIAN_POINT ( 'NONE',  ( -13.00000000000000178, 170.0000000000000000, 7.483314773547879106 ) ) ;
#8807 = CARTESIAN_POINT ( 'NONE',  ( 0.000000000000000000, 260.0000000000000000, 0.000000000000000000 ) ) ;
#8808 = EDGE_CURVE ( 'NONE', #9640, #4568, #9494, .T. ) ;
#8809 = SURFACE_STYLE_FILL_AREA ( #1527 ) ;
#8810 = CARTESIAN_POINT ( 'NONE',  ( 0.000000000000000000, 75.00000000000001421, 0.000000000000000000 ) ) ;
#8811 = ORIENTED_EDGE ( 'NONE', *, *, #8252, .T. ) ;
#8812 = VECTOR ( 'NONE', #3600, 1000.000000000000114 ) ;
#8813 = FILL_AREA_STYLE ('',( #2338 ) ) ;
#8814 = ADVANCED_FACE ( 'NONE', ( #7073 ), #7133, .T. ) ;
#8815 = CARTESIAN_POINT ( 'NONE',  ( -1.190781129305471087, 30.00000000000008882, 80.00000000000000000 ) ) ;
#8816 = DIRECTION ( 'NONE',  ( -0.000000000000000000, 1.000000000000000000, -0.000000000000000000 ) ) ;
#8817 = ORIENTED_EDGE ( 'NONE', *, *, #4266, .F. ) ;
#8818 = CARTESIAN_POINT ( 'NONE',  ( 74.91301266955075278, 17.04453457915816728, -24.03638115575044409 ) ) ;
#8819 = AXIS2_PLACEMENT_3D ( 'NONE', #10247, #10185, #6525 ) ;
#8820 = CIRCLE ( 'NONE', #675, 98.00000000000001421 ) ;
#8821 = CARTESIAN_POINT ( 'NONE',  ( -8.500000000000000000, 165.5000000000000000, 6.164414002968973350 ) ) ;
#8822 = ADVANCED_FACE ( 'NONE', ( #10052 ), #10997, .T. ) ;
#8823 = CARTESIAN_POINT ( 'NONE',  ( -1.915364268218909816, 111.9374999986344079, -1.915364268218909150 ) ) ;
#8824 = ORIENTED_EDGE ( 'NONE', *, *, #1223, .F. ) ;
#8825 = CYLINDRICAL_SURFACE ( 'NONE', #10144, 100.0000000000000284 ) ;
#8826 = ADVANCED_FACE ( 'NONE', ( #7195 ), #4303, .T. ) ;
#8827 = EDGE_CURVE ( 'NONE', #4808, #3422, #8118, .T. ) ;
#8828 = AXIS2_PLACEMENT_3D ( 'NONE', #10245, #2587, #3341 ) ;
#8829 = VECTOR ( 'NONE', #2166, 1000.000000000000000 ) ;
#8830 = ORIENTED_EDGE ( 'NONE', *, *, #4479, .T. ) ;
#8831 = CYLINDRICAL_SURFACE ( 'NONE', #12009, 17.50000000000000000 ) ;
#8832 = ORIENTED_EDGE ( 'NONE', *, *, #10642, .F. ) ;
#8833 = DIRECTION ( 'NONE',  ( 0.000000000000000000, 1.000000000000000000, 0.000000000000000000 ) ) ;
#8834 = CARTESIAN_POINT ( 'NONE',  ( 27.94372984915585789, 86.14533704847936235, 11.47449158599552455 ) ) ;
#8835 = VERTEX_POINT ( 'NONE', #6140 ) ;
#8836 = FACE_OUTER_BOUND ( 'NONE', #1363, .T. ) ;
#8837 = CARTESIAN_POINT ( 'NONE',  ( 72.61843774138907293, 50.00000000000000000, -18.75000000000000000 ) ) ;
#8838 = ORIENTED_EDGE ( 'NONE', *, *, #7891, .T. ) ;
#8839 = CARTESIAN_POINT ( 'NONE',  ( 1.658621287961228566E-16, 112.5624999986344079, 2.708734125000000326 ) ) ;
#8840 = VECTOR ( 'NONE', #5573, 1000.000000000000114 ) ;
#8841 = CARTESIAN_POINT ( 'NONE',  ( -3.250000000000000444, 114.3124999972688016, 1.346194077712559389 ) ) ;
#8842 = ORIENTED_EDGE ( 'NONE', *, *, #9513, .T. ) ;
#8843 = CARTESIAN_POINT ( 'NONE',  ( 0.000000000000000000, 115.0000000000000000, 0.000000000000000000 ) ) ;
#8844 = CARTESIAN_POINT ( 'NONE',  ( -25.00000000000000000, 345.0000000000000568, -90.00000000000000000 ) ) ;
#8845 = ORIENTED_EDGE ( 'NONE', *, *, #4258, .F. ) ;
#8846 = CIRCLE ( 'NONE', #6052, 3.250000000000000444 ) ;
#8847 = CARTESIAN_POINT ( 'NONE',  ( 7.344472908539098732, 24.78349364905406205, 79.50000000000000000 ) ) ;
#8848 = PLANE ( 'NONE',  #12076 ) ;
#8849 = EDGE_LOOP ( 'NONE', ( #8394, #1927, #60, #9862 ) ) ;
#8850 = CYLINDRICAL_SURFACE ( 'NONE', #10460, 35.00000000000000711 ) ;
#8851 = DIRECTION ( 'NONE',  ( 0.7071067811865513475, 0.7071067811865437980, 0.000000000000000000 ) ) ;
#8852 = CARTESIAN_POINT ( 'NONE',  ( -34.73110591274434000, 77.00000000000000000, 8.660254037844445918 ) ) ;
#8853 = ORIENTED_EDGE ( 'NONE', *, *, #2249, .T. ) ;
#8854 = DIRECTION ( 'NONE',  ( 0.7071067811865486830, -0.7071067811865464625, 0.000000000000000000 ) ) ;
#8855 = EDGE_CURVE ( 'NONE', #3002, #10848, #526, .T. ) ;
#8856 = CARTESIAN_POINT ( 'NONE',  ( 71.26020304811973460, 11.28911591861274744, 23.39373652035272144 ) ) ;
#8857 = AXIS2_PLACEMENT_3D ( 'NONE', #10760, #9939, #10943 ) ;
#8858 = EDGE_CURVE ( 'NONE', #9381, #3427, #10273, .T. ) ;
#8859 = MANIFOLD_SOLID_BREP ( 'Hex', #4093 ) ;
#8860 = AXIS2_PLACEMENT_3D ( 'NONE', #6220, #8488, #6570 ) ;
#8861 = AXIS2_PLACEMENT_3D ( 'NONE', #4347, #12029, #5357 ) ;
#8862 = ORIENTED_EDGE ( 'NONE', *, *, #11148, .F. ) ;
#8863 = DIRECTION ( 'NONE',  ( 0.000000000000000000, -0.000000000000000000, 1.000000000000000000 ) ) ;
#8864 = ORIENTED_EDGE ( 'NONE', *, *, #1928, .F. ) ;
#8865 = PRODUCT_DEFINITION_SHAPE ( 'NONE', 'NONE',  #12361 ) ;
#8866 = CARTESIAN_POINT ( 'NONE',  ( -0.9407811293054709756, 40.00000000000008527, 80.00000000000000000 ) ) ;
#8867 = CARTESIAN_POINT ( 'NONE',  ( -14.19078112930533209, 29.75000000000008882, 80.00000000000000000 ) ) ;
#8868 = ORIENTED_EDGE ( 'NONE', *, *, #7520, .F. ) ;
#8869 = CARTESIAN_POINT ( 'NONE',  ( -9.976035167149682081, 25.21650635094616533, 79.50000000000000000 ) ) ;
#8870 = DIRECTION ( 'NONE',  ( 0.000000000000000000, 0.000000000000000000, 1.000000000000000000 ) ) ;
#8871 = DIRECTION ( 'NONE',  ( -0.000000000000000000, -1.000000000000000000, -0.000000000000000000 ) ) ;
#8872 = CARTESIAN_POINT ( 'NONE',  ( 1.915364268218909594, 110.4374999986344079, 1.915364268218909594 ) ) ;
#8873 = VECTOR ( 'NONE', #8748, 1000.000000000000000 ) ;
#8874 = ADVANCED_FACE ( 'NONE', ( #4264 ), #9872, .F. ) ;
#8875 = ORIENTED_EDGE ( 'NONE', *, *, #2038, .F. ) ;
#8876 = SHAPE_REPRESENTATION ( 'Food Pusher', ( #1612 ), #9911 ) ;
#8877 = ORIENTED_EDGE ( 'NONE', *, *, #7943, .F. ) ;
#8878 = EDGE_CURVE ( 'NONE', #9534, #1174, #8279, .T. ) ;
#8879 = VECTOR ( 'NONE', #4569, 1000.000000000000000 ) ;
#8880 = PRESENTATION_STYLE_ASSIGNMENT (( #4214 ) ) ;
#8881 = CARTESIAN_POINT ( 'NONE',  ( 0.000000000000000000, 1.178949249685212974, -2.042000000000001148 ) ) ;
#8882 = CARTESIAN_POINT ( 'NONE',  ( 20.00000000000000355, 7.965803112215716020, -57.08203932499370836 ) ) ;
#8883 = DIRECTION ( 'NONE',  ( -0.6901483381584025967, 0.000000000000000000, -0.7236679289129753778 ) ) ;
#8884 = EDGE_CURVE ( 'NONE', #693, #3178, #7013, .T. ) ;
#8885 = CARTESIAN_POINT ( 'NONE',  ( -7.907287480251421030, 41.13333024919781167, 80.00000000000000000 ) ) ;
#8886 = CARTESIAN_POINT ( 'NONE',  ( 1.915364268218908927, 114.1874999986344079, -1.915364268218909816 ) ) ;
#8887 = EDGE_LOOP ( 'NONE', ( #11368, #4355, #7391, #1562 ) ) ;
#8888 = DIRECTION ( 'NONE',  ( 0.8660254037844362651, 0.000000000000000000, 0.5000000000000039968 ) ) ;
#8889 = VECTOR ( 'NONE', #10285, 1000.000000000000000 ) ;
#8890 = EDGE_CURVE ( 'NONE', #5487, #10768, #9078, .T. ) ;
#8891 = ORIENTED_EDGE ( 'NONE', *, *, #10112, .F. ) ;
#8892 = DIRECTION ( 'NONE',  ( -0.000000000000000000, -1.000000000000000000, -0.000000000000000000 ) ) ;
#8893 = ORIENTED_EDGE ( 'NONE', *, *, #4807, .T. ) ;
#8894 = CARTESIAN_POINT ( 'NONE',  ( 0.000000000000000000, 110.0000000000000000, 3.250000000000000444 ) ) ;
#8895 = DIRECTION ( 'NONE',  ( 0.000000000000000000, 0.000000000000000000, 1.000000000000000000 ) ) ;
#8896 = EDGE_LOOP ( 'NONE', ( #7842, #10292, #4607, #4746 ) ) ;
#8897 = CARTESIAN_POINT ( 'NONE',  ( 27.33018067101282966, 87.00000000000000000, 12.37179148263486539 ) ) ;
#8898 = DIRECTION ( 'NONE',  ( 0.000000000000000000, 0.000000000000000000, -1.000000000000000000 ) ) ;
#8899 = EDGE_CURVE ( 'NONE', #9385, #9969, #5320, .T. ) ;
#8900 = EDGE_CURVE ( 'NONE', #8617, #3205, #11759, .T. ) ;
#8901 = ORIENTED_EDGE ( 'NONE', *, *, #9547, .T. ) ;
#8902 = LINE ( 'NONE', #9082, #4579 ) ;
#8903 = ORIENTED_EDGE ( 'NONE', *, *, #8954, .F. ) ;
#8904 = DIRECTION ( 'NONE',  ( -0.000000000000000000, -0.000000000000000000, 1.000000000000000000 ) ) ;
#8905 = DIRECTION ( 'NONE',  ( 0.000000000000000000, 0.000000000000000000, 1.000000000000000000 ) ) ;
#8906 = ORIENTED_EDGE ( 'NONE', *, *, #1891, .T. ) ;
#8907 = CARTESIAN_POINT ( 'NONE',  ( 0.000000000000000000, -5.000000000000000000, 0.000000000000000000 ) ) ;
#8908 = LINE ( 'NONE', #374, #8273 ) ;
#8909 = VECTOR ( 'NONE', #9210, 1000.000000000000000 ) ;
#8910 = ORIENTED_EDGE ( 'NONE', *, *, #10258, .T. ) ;
#8911 = CARTESIAN_POINT ( 'NONE',  ( -20.00000000000000355, 50.00000000000000000, -57.08203932499370836 ) ) ;
#8912 = CARTESIAN_POINT ( 'NONE',  ( 0.000000000000000000, 285.0000000000000568, 0.000000000000000000 ) ) ;
#8913 = DIRECTION ( 'NONE',  ( -1.000000000000000000, -0.000000000000000000, -0.000000000000000000 ) ) ;
#8914 = ORIENTED_EDGE ( 'NONE', *, *, #11292, .F. ) ;
#8915 = FACE_OUTER_BOUND ( 'NONE', #1555, .T. ) ;
#8916 = CARTESIAN_POINT ( 'NONE',  ( 70.03799559100536953, 14.91291538047573439, 26.82731484558927093 ) ) ;
#8917 = FACE_OUTER_BOUND ( 'NONE', #2170, .T. ) ;
#8918 = EDGE_LOOP ( 'NONE', ( #6193, #479, #6064, #5044, #8483, #11550 ) ) ;
#8919 = CARTESIAN_POINT ( 'NONE',  ( 76.05876219242703939, 15.60447527335573703, 22.40335076292606331 ) ) ;
#8920 = CARTESIAN_POINT ( 'NONE',  ( 69.87020289360394543, 44.20576086388582127, -27.26117375607963922 ) ) ;
#8921 = VERTEX_POINT ( 'NONE', #11883 ) ;
#8922 = ADVANCED_FACE ( 'NONE', ( #585 ), #10174, .T. ) ;
#8923 = CARTESIAN_POINT ( 'NONE',  ( -31.74999999999995737, 3.061616997868383634E-16, -2.500000000000000444 ) ) ;
#8924 = EDGE_CURVE ( 'NONE', #2786, #8477, #10238, .T. ) ;
#8925 = CARTESIAN_POINT ( 'NONE',  ( 71.59683363033870762, 44.46727110088187374, 22.47949853503603990 ) ) ;
#8926 = EDGE_LOOP ( 'NONE', ( #1531, #1188, #7655 ) ) ;
#8927 = CARTESIAN_POINT ( 'NONE',  ( -1.440781129305261477, 20.00000000000009592, 80.00000000000000000 ) ) ;
#8928 = CARTESIAN_POINT ( 'NONE',  ( -2.298097038856279362, 112.2499999972688158, 2.298097038856279806 ) ) ;
#8929 = DIRECTION ( 'NONE',  ( -0.000000000000000000, -1.000000000000000000, -0.000000000000000000 ) ) ;
#8930 = EDGE_CURVE ( 'NONE', #4639, #592, #1925, .T. ) ;
#8931 = VERTEX_POINT ( 'NONE', #4383 ) ;
#8932 = VERTEX_POINT ( 'NONE', #11062 ) ;
#8933 = VERTEX_POINT ( 'NONE', #3522 ) ;
#8934 = AXIS2_PLACEMENT_3D ( 'NONE', #3301, #7163, #10023 ) ;
#8935 = AXIS2_PLACEMENT_3D ( 'NONE', #2, #187, #1073 ) ;
#8936 = COLOUR_RGB ( '', 0.31764706, 0.68627451, 0.89019608) ;
#8937 = LINE ( 'NONE', #1287, #6087 ) ;
#8938 = DIRECTION ( 'NONE',  ( 0.9682458365518543664, 0.000000000000000000, -0.2499999999999996947 ) ) ;
#8939 = CARTESIAN_POINT ( 'NONE',  ( 0.000000000000000000, 77.00000000000000000, 0.000000000000000000 ) ) ;
#8940 = DIRECTION ( 'NONE',  ( -0.000000000000000000, -1.000000000000000000, -0.000000000000000000 ) ) ;
#8941 = CARTESIAN_POINT ( 'NONE',  ( 140.0000000000011369, 67.07106781186550393, 25.00000000000000000 ) ) ;
#8942 = LINE ( 'NONE', #9882, #9630 ) ;
#8943 = CARTESIAN_POINT ( 'NONE',  ( 1.121994411437819528, 113.1249999986343937, -2.708734124999999882 ) ) ;
#8944 = VERTEX_POINT ( 'NONE', #11124 ) ;
#8945 = FACE_OUTER_BOUND ( 'NONE', #10973, .T. ) ;
#8946 = ORIENTED_EDGE ( 'NONE', *, *, #11700, .F. ) ;
#8947 = VECTOR ( 'NONE', #6467, 1000.000000000000000 ) ;
#8948 = CARTESIAN_POINT ( 'NONE',  ( 27.53586651884002734, 87.45908356336218503, 11.91741659355933791 ) ) ;
#8949 = ORIENTED_EDGE ( 'NONE', *, *, #8293, .F. ) ;
#8950 = VECTOR ( 'NONE', #1660, 1000.000000000000000 ) ;
#8951 = DIRECTION ( 'NONE',  ( 0.000000000000000000, 0.000000000000000000, 1.000000000000000000 ) ) ;
#8952 = DIRECTION ( 'NONE',  ( 0.000000000000000000, 0.000000000000000000, -1.000000000000000000 ) ) ;
#8953 = VERTEX_POINT ( 'NONE', #12250 ) ;
#8954 = EDGE_CURVE ( 'NONE', #7578, #1095, #3695, .T. ) ;
#8955 = DIRECTION ( 'NONE',  ( 0.000000000000000000, 0.000000000000000000, 1.000000000000000000 ) ) ;
#8956 = CARTESIAN_POINT ( 'NONE',  ( -31.69148534550512863, 87.00819463772765516, -8.674447566738409776 ) ) ;
#8957 = ORIENTED_EDGE ( 'NONE', *, *, #10206, .T. ) ;
#8958 = CARTESIAN_POINT ( 'NONE',  ( 1.990051048614449116E-16, 113.2500000000000000, 3.250000000000000444 ) ) ;
#8959 = CIRCLE ( 'NONE', #3599, 5.000000000000000888 ) ;
#8960 = ORIENTED_EDGE ( 'NONE', *, *, #832, .F. ) ;
#8961 = VECTOR ( 'NONE', #2042, 1000.000000000000000 ) ;
#8962 = ADVANCED_FACE ( 'NONE', ( #10363 ), #9107, .F. ) ;
#8963 = CARTESIAN_POINT ( 'NONE',  ( 1.224646799147353533E-14, 285.0000000000000568, -100.0000000000000284 ) ) ;
#8964 = CARTESIAN_POINT ( 'NONE',  ( 28.72281323269012532, 87.00000000000000000, 8.660254037844435260 ) ) ;
#8965 = EDGE_CURVE ( 'NONE', #7898, #2259, #8181, .T. ) ;
#8966 = EDGE_LOOP ( 'NONE', ( #9203, #7501, #4348, #11296 ) ) ;
#8967 = DIRECTION ( 'NONE',  ( 0.000000000000000000, 1.000000000000000000, 0.000000000000000000 ) ) ;
#8968 = CARTESIAN_POINT ( 'NONE',  ( 4.163799117101000559E-16, 109.0000000000000000, -3.399999999999999911 ) ) ;
#8969 = AXIS2_PLACEMENT_3D ( 'NONE', #1066, #11666, #3118 ) ;
#8970 = EDGE_LOOP ( 'NONE', ( #11497, #6732 ) ) ;
#8971 = FACE_OUTER_BOUND ( 'NONE', #11001, .T. ) ;
#8972 = CARTESIAN_POINT ( 'NONE',  ( 74.16198487095665826, 40.00000000000009237, -25.00000000000000000 ) ) ;
#8973 = DIRECTION ( 'NONE',  ( -0.000000000000000000, -0.000000000000000000, 1.000000000000000000 ) ) ;
#8974 = VERTEX_POINT ( 'NONE', #2578 ) ;
#8975 = CARTESIAN_POINT ( 'NONE',  ( 82.90657655638969459, 275.0000000000000000, 79.06642500897268633 ) ) ;
#8976 = VECTOR ( 'NONE', #6460, 1000.000000000000114 ) ;
#8977 = CARTESIAN_POINT ( 'NONE',  ( 74.21645788709501801, 19.16431193171542802, 24.93253696209799131 ) ) ;
#8978 = ADVANCED_BREP_SHAPE_REPRESENTATION ( '', ( #461, #1612 ), #1360 ) ;
#8979 = VECTOR ( 'NONE', #54, 1000.000000000000000 ) ;
#8980 = VERTEX_POINT ( 'NONE', #11314 ) ;
#8981 = ADVANCED_FACE ( 'NONE', ( #10108 ), #9235, .T. ) ;
#8982 = DIRECTION ( 'NONE',  ( 0.000000000000000000, 1.000000000000000000, 0.000000000000000000 ) ) ;
#8983 = EDGE_CURVE ( 'NONE', #5612, #12245, #1535, .T. ) ;
#8984 = FACE_OUTER_BOUND ( 'NONE', #1640, .T. ) ;
#8985 = ORIENTED_EDGE ( 'NONE', *, *, #11441, .F. ) ;
#8986 = DIRECTION ( 'NONE',  ( 0.000000000000000000, 0.000000000000000000, 1.000000000000000000 ) ) ;
#8987 = CARTESIAN_POINT ( 'NONE',  ( 74.16198487095664404, 40.00000000000009237, 25.00000000000000000 ) ) ;
#8988 = ORIENTED_EDGE ( 'NONE', *, *, #10339, .F. ) ;
#8989 = CARTESIAN_POINT ( 'NONE',  ( 0.000000000000000000, 65.00000000000000000, 25.00000000000000000 ) ) ;
#8990 = LINE ( 'NONE', #10871, #9731 ) ;
#8991 = DIRECTION ( 'NONE',  ( 0.4999999999999914513, -0.8660254037844435926, 0.000000000000000000 ) ) ;
#8992 = ORIENTED_EDGE ( 'NONE', *, *, #7034, .F. ) ;
#8993 = ORIENTED_EDGE ( 'NONE', *, *, #6848, .T. ) ;
#8994 = VERTEX_POINT ( 'NONE', #11252 ) ;
#8995 = SURFACE_SIDE_STYLE ('',( #6902 ) ) ;
#8996 = LINE ( 'NONE', #7269, #11924 ) ;
#8997 = CARTESIAN_POINT ( 'NONE',  ( 165.0000000000011369, 225.0000000000000853, 20.00000000000000000 ) ) ;
#8998 = DIRECTION ( 'NONE',  ( 0.8660254037844434816, 0.4999999999999913958, 0.000000000000000000 ) ) ;
#8999 = DIRECTION ( 'NONE',  ( -0.000000000000000000, -1.000000000000000000, -0.000000000000000000 ) ) ;
#9000 = LINE ( 'NONE', #8007, #1119 ) ;
#9001 = DIRECTION ( 'NONE',  ( 0.7071067811865495711, 0.7071067811865455743, -0.000000000000000000 ) ) ;
#9002 = DIRECTION ( 'NONE',  ( 0.000000000000000000, 0.000000000000000000, -1.000000000000000000 ) ) ;
#9003 = CARTESIAN_POINT ( 'NONE',  ( -1.121994411437820416, 113.9999999986343937, -2.708734124999999882 ) ) ;
#9004 = VECTOR ( 'NONE', #8463, 1000.000000000000000 ) ;
#9005 = ORIENTED_EDGE ( 'NONE', *, *, #9929, .F. ) ;
#9006 = CARTESIAN_POINT ( 'NONE',  ( 0.2500000000000002220, 0.000000000000000000, 0.000000000000000000 ) ) ;
#9007 = EDGE_CURVE ( 'NONE', #5882, #2768, #2760, .T. ) ;
#9008 = EDGE_LOOP ( 'NONE', ( #11105, #6939 ) ) ;
#9009 = AXIS2_PLACEMENT_3D ( 'NONE', #10758, #1411, #3408 ) ;
#9010 = FACE_OUTER_BOUND ( 'NONE', #6180, .T. ) ;
#9011 = ORIENTED_EDGE ( 'NONE', *, *, #11916, .T. ) ;
#9012 = DIRECTION ( 'NONE',  ( 0.000000000000000000, 0.000000000000000000, 1.000000000000000000 ) ) ;
#9013 = LINE ( 'NONE', #10019, #4094 ) ;
#9014 = ORIENTED_EDGE ( 'NONE', *, *, #9888, .T. ) ;
#9015 = DIRECTION ( 'NONE',  ( 1.224646799147351482E-16, 0.000000000000000000, -1.000000000000000000 ) ) ;
#9016 = FACE_OUTER_BOUND ( 'NONE', #6362, .T. ) ;
#9017 = ITEM_DEFINED_TRANSFORMATION ( 'NONE', 'NONE', #8325,  #1612 ) ;
#9018 = ORIENTED_EDGE ( 'NONE', *, *, #9794, .F. ) ;
#9019 = CARTESIAN_POINT ( 'NONE',  ( 71.66825662749599246, 49.34246535461046790, -22.10769995529665977 ) ) ;
#9020 = PRESENTATION_LAYER_ASSIGNMENT (  '', '', ( #1671 ) ) ;
#9021 = CIRCLE ( 'NONE', #7453, 30.00000000000000711 ) ;
#9022 = EDGE_CURVE ( 'NONE', #9041, #1734, #8245, .T. ) ;
#9023 = EDGE_CURVE ( 'NONE', #1518, #5644, #10688, .T. ) ;
#9024 = VERTEX_POINT ( 'NONE', #7325 ) ;
#9025 = CARTESIAN_POINT ( 'NONE',  ( 31.23312648697674732, 87.04033007153441304, 8.730107770814976575 ) ) ;
#9026 = CARTESIAN_POINT ( 'NONE',  ( 0.000000000000000000, 122.0000000000000000, 0.000000000000000000 ) ) ;
#9027 = ORIENTED_EDGE ( 'NONE', *, *, #6008, .F. ) ;
#9028 = CARTESIAN_POINT ( 'NONE',  ( 0.000000000000000000, 165.0000000000000000, -9.999999999999998224 ) ) ;
#9029 = CARTESIAN_POINT ( 'NONE',  ( -20.00000000000000355, 65.00000000000000000, 57.08203932499370836 ) ) ;
#9030 = VERTEX_POINT ( 'NONE', #3577 ) ;
#9031 = VECTOR ( 'NONE', #3040, 1000.000000000000000 ) ;
#9032 = CARTESIAN_POINT ( 'NONE',  ( 0.000000000000000000, 50.00000000000000000, 0.000000000000000000 ) ) ;
#9033 = DIRECTION ( 'NONE',  ( -3.469446951953613203E-16, 0.000000000000000000, -1.000000000000000000 ) ) ;
#9034 = VERTEX_POINT ( 'NONE', #7387 ) ;
#9035 = CARTESIAN_POINT ( 'NONE',  ( 1.346194077712572934, 111.8124999999999858, -3.249999999999987121 ) ) ;
#9036 = CARTESIAN_POINT ( 'NONE',  ( 70.29663099721912545, 13.81758329365315063, 26.14423569115638912 ) ) ;
#9037 = EDGE_CURVE ( 'NONE', #108, #1744, #12289, .T. ) ;
#9038 = EDGE_CURVE ( 'NONE', #4568, #6913, #9296, .T. ) ;
#9039 = AXIS2_PLACEMENT_3D ( 'NONE', #4109, #11907, #9955 ) ;
#9040 = AXIS2_PLACEMENT_3D ( 'NONE', #9660, #11617, #8726 ) ;
#9041 = VERTEX_POINT ( 'NONE', #9357 ) ;
#9042 = DIRECTION ( 'NONE',  ( -0.000000000000000000, -0.000000000000000000, 1.000000000000000000 ) ) ;
#9043 = PLANE ( 'NONE',  #9435 ) ;
#9044 = VERTEX_POINT ( 'NONE', #7446 ) ;
#9045 = CARTESIAN_POINT ( 'NONE',  ( -8.000000000000000000, 165.0000000000000000, -5.999999999999998224 ) ) ;
#9046 = CARTESIAN_POINT ( 'NONE',  ( 69.52686081700198883, 40.67794899483754278, 28.12499999881304191 ) ) ;
#9047 = ORIENTED_EDGE ( 'NONE', *, *, #6697, .F. ) ;
#9048 = CARTESIAN_POINT ( 'NONE',  ( -5.999999999999999112, 50.00000000000000000, 60.00000000000002132 ) ) ;
#9049 = DIRECTION ( 'NONE',  ( 0.000000000000000000, 1.000000000000000000, 0.000000000000000000 ) ) ;
#9050 = DIRECTION ( 'NONE',  ( -0.8660254037844363761, 0.5000000000000038858, 0.000000000000000000 ) ) ;
#9051 = LINE ( 'NONE', #5457, #3201 ) ;
#9052 = VECTOR ( 'NONE', #6002, 1000.000000000000000 ) ;
#9053 = EDGE_CURVE ( 'NONE', #9749, #11846, #2524, .T. ) ;
#9054 = EDGE_CURVE ( 'NONE', #9195, #3744, #4632, .T. ) ;
#9055 = ORIENTED_EDGE ( 'NONE', *, *, #4420, .T. ) ;
#9056 =( NAMED_UNIT ( * ) PLANE_ANGLE_UNIT ( ) SI_UNIT ( $, .RADIAN. ) );
#9057 = ORIENTED_EDGE ( 'NONE', *, *, #4838, .T. ) ;
#9058 = AXIS2_PLACEMENT_3D ( 'NONE', #6120, #9971, #6179 ) ;
#9059 = DIRECTION ( 'NONE',  ( 0.000000000000000000, 0.000000000000000000, 1.000000000000000000 ) ) ;
#9060 = CARTESIAN_POINT ( 'NONE',  ( 8.817456953860944867E-15, 67.00000000000000000, 72.00000000000002842 ) ) ;
#9061 = DIRECTION ( 'NONE',  ( 0.000000000000000000, -0.000000000000000000, 1.000000000000000000 ) ) ;
#9062 = AXIS2_PLACEMENT_3D ( 'NONE', #1852, #10265, #1792 ) ;
#9063 = CARTESIAN_POINT ( 'NONE',  ( -0.9407811293052825707, 17.00000000000008882, 79.50000000000000000 ) ) ;
#9064 = DIRECTION ( 'NONE',  ( -0.000000000000000000, -1.000000000000000000, -0.000000000000000000 ) ) ;
#9065 = CARTESIAN_POINT ( 'NONE',  ( 0.000000000000000000, 115.0000000000000000, 0.000000000000000000 ) ) ;
#9066 = CARTESIAN_POINT ( 'NONE',  ( 2.708734125000000326, 111.3124999986344079, 0.000000000000000000 ) ) ;
#9067 = CARTESIAN_POINT ( 'NONE',  ( 1.658621287961228320E-16, 110.8124999986344079, 2.708734124999999882 ) ) ;
#9068 = CARTESIAN_POINT ( 'NONE',  ( 90.45849111412074706, 275.0000000000000000, 86.26854226980164242 ) ) ;
#9069 = AXIS2_PLACEMENT_3D ( 'NONE', #4218, #6962, #4333 ) ;
#9070 = EDGE_LOOP ( 'NONE', ( #6115, #7966, #10518, #6610 ) ) ;
#9071 = DIRECTION ( 'NONE',  ( -0.000000000000000000, -1.000000000000000000, -0.000000000000000000 ) ) ;
#9072 = VERTEX_POINT ( 'NONE', #10 ) ;
#9073 = ADVANCED_FACE ( 'NONE', ( #3074 ), #4008, .F. ) ;
#9074 = EDGE_CURVE ( 'NONE', #10619, #10742, #9681, .T. ) ;
#9075 = DIRECTION ( 'NONE',  ( -1.000000000000000000, 0.000000000000000000, 0.000000000000000000 ) ) ;
#9076 = ORIENTED_EDGE ( 'NONE', *, *, #1595, .F. ) ;
#9077 = CARTESIAN_POINT ( 'NONE',  ( 0.000000000000000000, 153.0000000000000000, 0.000000000000000000 ) ) ;
#9078 = CIRCLE ( 'NONE', #11094, 70.00000000000001421 ) ;
#9079 = DIRECTION ( 'NONE',  ( -0.000000000000000000, -1.000000000000000000, 0.000000000000000000 ) ) ;
#9080 = EDGE_CURVE ( 'NONE', #3926, #834, #2884, .T. ) ;
#9081 = VERTEX_POINT ( 'NONE', #194 ) ;
#9082 = CARTESIAN_POINT ( 'NONE',  ( 150.0000000000010800, 15.00000000000008882, -19.99999999999999645 ) ) ;
#9083 = ORIENTED_EDGE ( 'NONE', *, *, #1222, .F. ) ;
#9084 = CARTESIAN_POINT ( 'NONE',  ( 0.000000000000000000, 127.0000000000000000, 0.000000000000000000 ) ) ;
#9085 = DIRECTION ( 'NONE',  ( 1.000000000000000000, 0.000000000000000000, -0.000000000000000000 ) ) ;
#9086 = ORIENTED_EDGE ( 'NONE', *, *, #1256, .T. ) ;
#9087 = VERTEX_POINT ( 'NONE', #71 ) ;
#9088 = DIRECTION ( 'NONE',  ( 0.000000000000000000, 0.000000000000000000, 1.000000000000000000 ) ) ;
#9089 = CARTESIAN_POINT ( 'NONE',  ( 72.28523001630050260, 10.06812071389296293, 20.00612389586592954 ) ) ;
#9090 = ORIENTED_EDGE ( 'NONE', *, *, #11424, .T. ) ;
#9091 = DIRECTION ( 'NONE',  ( 0.000000000000000000, 0.000000000000000000, -1.000000000000000000 ) ) ;
#9092 = CARTESIAN_POINT ( 'NONE',  ( -27.32050286291078933, 86.95679894682507438, -12.39317045950328477 ) ) ;
#9093 = LINE ( 'NONE', #9914, #6590 ) ;
#9094 = ORIENTED_EDGE ( 'NONE', *, *, #27, .T. ) ;
#9095 = FACE_OUTER_BOUND ( 'NONE', #1947, .T. ) ;
#9096 = CARTESIAN_POINT ( 'NONE',  ( 74.16874958671132845, 19.66594046503222515, 24.99164682819348471 ) ) ;
#9097 = ORIENTED_EDGE ( 'NONE', *, *, #11041, .F. ) ;
#9098 = CIRCLE ( 'NONE', #10904, 14.99999999999999822 ) ;
#9099 = ADVANCED_FACE ( 'NONE', ( #9667 ), #3888, .T. ) ;
#9100 = CARTESIAN_POINT ( 'NONE',  ( 77.45966692414835109, 45.00000000000009237, -20.00000000000000355 ) ) ;
#9101 = CARTESIAN_POINT ( 'NONE',  ( 74.16198487095665826, 20.00000000000009237, 30.00000000000000355 ) ) ;
#9102 = ORIENTED_EDGE ( 'NONE', *, *, #368, .F. ) ;
#9103 = PLANE ( 'NONE',  #1090 ) ;
#9104 = CARTESIAN_POINT ( 'NONE',  ( 70.80917463421374691, 40.85568721397550007, 24.94686153084717617 ) ) ;
#9105 = ORIENTED_EDGE ( 'NONE', *, *, #8011, .T. ) ;
#9106 = CARTESIAN_POINT ( 'NONE',  ( 11.80921887069467324, 30.25000000000018474, 79.50000000000000000 ) ) ;
#9107 = PLANE ( 'NONE',  #12089 ) ;
#9108 = CARTESIAN_POINT ( 'NONE',  ( -2.708734125000000770, 112.8749999986344079, -1.121994411437818639 ) ) ;
#9109 = ADVANCED_FACE ( 'NONE', ( #899 ), #10423, .T. ) ;
#9110 = AXIS2_PLACEMENT_3D ( 'NONE', #1410, #10002, #3407 ) ;
#9111 = AXIS2_PLACEMENT_3D ( 'NONE', #11232, #5500, #11355 ) ;
#9112 = VERTEX_POINT ( 'NONE', #12308 ) ;
#9113 = ORIENTED_EDGE ( 'NONE', *, *, #8115, .T. ) ;
#9114 = UNCERTAINTY_MEASURE_WITH_UNIT (LENGTH_MEASURE( 1.000000000000000082E-05 ), #3339, 'distance_accuracy_value', 'NONE');
#9115 = CYLINDRICAL_SURFACE ( 'NONE', #7640, 72.00000000000002842 ) ;
#9116 = CARTESIAN_POINT ( 'NONE',  ( 2.500000000000000000, 2.357898499370431722, -2.818925648462311528E-15 ) ) ;
#9117 = ADVANCED_FACE ( 'NONE', ( #7684 ), #11889, .T. ) ;
#9118 = CARTESIAN_POINT ( 'NONE',  ( -24.99999999999999289, 450.0000000000000568, -14.99999999999999289 ) ) ;
#9119 = FACE_OUTER_BOUND ( 'NONE', #8370, .T. ) ;
#9120 = EDGE_CURVE ( 'NONE', #7233, #11110, #5721, .T. ) ;
#9121 = CARTESIAN_POINT ( 'NONE',  ( -27.31068353816013783, 86.91310272383458368, -12.41479448187959278 ) ) ;
#9122 = CARTESIAN_POINT ( 'NONE',  ( 30.07733313487553772, 77.00000000000709122, -4.660254037819535178 ) ) ;
#9123 = CARTESIAN_POINT ( 'NONE',  ( 13.80921887069452758, 30.00000000000009237, 73.71774192269630532 ) ) ;
#9124 = DIRECTION ( 'NONE',  ( -0.000000000000000000, 1.000000000000000000, -0.000000000000000000 ) ) ;
#9125 = DIRECTION ( 'NONE',  ( 1.224646799147352961E-16, 0.000000000000000000, -1.000000000000000000 ) ) ;
#9126 = AXIS2_PLACEMENT_3D ( 'NONE', #3791, #1981, #9635 ) ;
#9127 = VECTOR ( 'NONE', #1197, 1000.000000000000000 ) ;
#9128 = EDGE_CURVE ( 'NONE', #5113, #9199, #7809, .T. ) ;
#9129 = CYLINDRICAL_SURFACE ( 'NONE', #9378, 9.999999999999994671 ) ;
#9130 = ORIENTED_EDGE ( 'NONE', *, *, #3582, .F. ) ;
#9131 = CARTESIAN_POINT ( 'NONE',  ( 27.67946139862178256, 88.39098822669899391, 11.04733141613932190 ) ) ;
#9132 = ORIENTED_EDGE ( 'NONE', *, *, #7536, .F. ) ;
#9133 = CYLINDRICAL_SURFACE ( 'NONE', #5092, 22.00000000000000355 ) ;
#9134 = DIRECTION ( 'NONE',  ( -0.000000000000000000, 1.000000000000000000, -0.000000000000000000 ) ) ;
#9135 = ORIENTED_EDGE ( 'NONE', *, *, #11312, .T. ) ;
#9136 = CIRCLE ( 'NONE', #3775, 70.00000000000001421 ) ;
#9137 = CARTESIAN_POINT ( 'NONE',  ( -7.474274778359198734, 41.38333024919781167, 80.00000000000000000 ) ) ;
#9138 = AXIS2_PLACEMENT_3D ( 'NONE', #10614, #9669, #1148 ) ;
#9139 = CARTESIAN_POINT ( 'NONE',  ( -32.15778161310143446, 87.00000000000000000, -8.660254037844435260 ) ) ;
#9140 = ORIENTED_EDGE ( 'NONE', *, *, #3609, .T. ) ;
#9141 = LINE ( 'NONE', #6171, #10349 ) ;
#9142 = EDGE_CURVE ( 'NONE', #10836, #3922, #1887, .T. ) ;
#9143 = PRODUCT_RELATED_PRODUCT_CATEGORY ( 'part', '', ( #207 ) ) ;
#9144 = EDGE_CURVE ( 'NONE', #12045, #8921, #4712, .T. ) ;
#9145 = AXIS2_PLACEMENT_3D ( 'NONE', #9376, #7406, #10257 ) ;
#9146 = ORIENTED_EDGE ( 'NONE', *, *, #6256, .T. ) ;
#9147 = CARTESIAN_POINT ( 'NONE',  ( -12.44911137850304250, 36.50000000000007816, 80.00000000000000000 ) ) ;
#9148 = DIRECTION ( 'NONE',  ( -0.000000000000000000, 1.000000000000000000, -0.000000000000000000 ) ) ;
#9149 = ORIENTED_EDGE ( 'NONE', *, *, #5631, .F. ) ;
#9150 = CARTESIAN_POINT ( 'NONE',  ( -18.80690714323172941, 285.0000000000000568, -123.5771024247852665 ) ) ;
#9151 = CARTESIAN_POINT ( 'NONE',  ( -25.00000000000000000, 347.0000000000000568, -59.99999999999999289 ) ) ;
#9152 = ORIENTED_EDGE ( 'NONE', *, *, #2974, .F. ) ;
#9153 = CARTESIAN_POINT ( 'NONE',  ( 0.000000000000000000, 67.00000000000000000, 0.000000000000000000 ) ) ;
#9155 = DIRECTION ( 'NONE',  ( 0.5000000000000016653, 0.8660254037844378194, 0.000000000000000000 ) ) ;
#9154 = VECTOR ( 'NONE', #195, 1000.000000000000000 ) ;
#9156 = DIRECTION ( 'NONE',  ( 1.564230817409691233E-15, 0.000000000000000000, -1.000000000000000000 ) ) ;
#9157 =( GEOMETRIC_REPRESENTATION_CONTEXT ( 3 ) GLOBAL_UNCERTAINTY_ASSIGNED_CONTEXT ( ( #1534 ) ) GLOBAL_UNIT_ASSIGNED_CONTEXT ( ( #1039, #4840, #6900 ) ) REPRESENTATION_CONTEXT ( 'NONE', 'WORKASPACE' ) );
#9158 = ORIENTED_EDGE ( 'NONE', *, *, #9144, .F. ) ;
#9159 = DIRECTION ( 'NONE',  ( -1.000000000000000000, 0.000000000000000000, -0.000000000000000000 ) ) ;
#9160 = CARTESIAN_POINT ( 'NONE',  ( -1.440781129305261477, 20.00000000000009592, 79.50000000000000000 ) ) ;
#9161 = ADVANCED_FACE ( 'NONE', ( #3949 ), #2950, .F. ) ;
#9162 = AXIS2_PLACEMENT_3D ( 'NONE', #1635, #7547, #4737 ) ;
#9163 = ORIENTED_EDGE ( 'NONE', *, *, #5971, .F. ) ;
#9164 = CARTESIAN_POINT ( 'NONE',  ( -25.00000000000000000, 570.2996408614167194, -31.99999999999999289 ) ) ;
#9165 = FACE_OUTER_BOUND ( 'NONE', #5214, .T. ) ;
#9166 = ORIENTED_EDGE ( 'NONE', *, *, #10820, .T. ) ;
#9167 = CARTESIAN_POINT ( 'NONE',  ( 0.000000000000000000, 225.0000000000000853, -25.00000000000000000 ) ) ;
#9168 = CARTESIAN_POINT ( 'NONE',  ( -0.9407811293052825707, 17.00000000000008882, 79.50000000000000000 ) ) ;
#9169 = EDGE_LOOP ( 'NONE', ( #28, #2196, #5145, #6477 ) ) ;
#9170 = DIRECTION ( 'NONE',  ( 0.000000000000000000, 1.000000000000000000, 0.000000000000000000 ) ) ;
#9171 = DIRECTION ( 'NONE',  ( -0.000000000000000000, -1.000000000000000000, -0.000000000000000000 ) ) ;
#9172 = CARTESIAN_POINT ( 'NONE',  ( -4.975863863883684959E-16, 114.0624999986344079, -2.708734125000000326 ) ) ;
#9173 = TOROIDAL_SURFACE ( 'NONE', #7968, 65.00000000000001421, 5.000000000000000000 ) ;
#9174 = CARTESIAN_POINT ( 'NONE',  ( 1.915364268218908705, 112.4374999986344079, -1.915364268218909594 ) ) ;
#9175 =( BOUNDED_CURVE ( )  B_SPLINE_CURVE ( 2, ( #5666, #10452, #6776, #2784, #9571, #35, #3037, #11463, #12275 ),
 .UNSPECIFIED., .F., .F. ) 
 B_SPLINE_CURVE_WITH_KNOTS ( ( 3, 2, 2, 2, 3 ),
 ( 0.6875000000000005551, 0.7187500000000005551, 0.7500000000000006661, 0.7812500000000006661, 0.8125000000000006661 ),
 .UNSPECIFIED. ) 
 CURVE ( )  GEOMETRIC_REPRESENTATION_ITEM ( )  RATIONAL_B_SPLINE_CURVE ( ( 0.9999999999999986677, 0.9238795325112880708, 1.000000000000000000, 0.9238795325112867385, 1.000000000000000000, 0.9238795325112867385, 1.000000000000000000, 0.9238795325112850731, 1.000000000000001554 ) ) 
 REPRESENTATION_ITEM ( '' )  );
#9176 = VECTOR ( 'NONE', #801, 999.9999999999997726 ) ;
#9177 = ORIENTED_EDGE ( 'NONE', *, *, #8769, .F. ) ;
#9178 = VERTEX_POINT ( 'NONE', #134 ) ;
#9179 = EDGE_CURVE ( 'NONE', #5710, #7734, #6692, .T. ) ;
#9180 = DIRECTION ( 'NONE',  ( 0.000000000000000000, 0.000000000000000000, -1.000000000000000000 ) ) ;
#9181 = EDGE_CURVE ( 'NONE', #861, #9835, #11558, .T. ) ;
#9182 = CARTESIAN_POINT ( 'NONE',  ( -30.12465603153679439, 85.44772375131798015, -9.971632707744779722 ) ) ;
#9183 = DIRECTION ( 'NONE',  ( -0.7071067811865511255, -0.7071067811865440200, 9.813077866773545180E-16 ) ) ;
#9184 = FACE_OUTER_BOUND ( 'NONE', #3732, .T. ) ;
#9185 = CARTESIAN_POINT ( 'NONE',  ( -27.67946139862177546, 88.39098822669897970, -11.04733141613932901 ) ) ;
#9186 = CARTESIAN_POINT ( 'NONE',  ( 1.836970198721029589E-15, 216.0365690573663926, 15.00000000000000000 ) ) ;
#9187 = DIRECTION ( 'NONE',  ( -0.000000000000000000, -0.000000000000000000, 1.000000000000000000 ) ) ;
#9188 = CARTESIAN_POINT ( 'NONE',  ( 70.26686370603788134, 13.95206716814361236, -26.22231631056802925 ) ) ;
#9189 = CARTESIAN_POINT ( 'NONE',  ( -1.346194077712560944, 112.6874999999999858, -3.249999999999999556 ) ) ;
#9190 = FACE_OUTER_BOUND ( 'NONE', #3898, .T. ) ;
#9191 = AXIS2_PLACEMENT_3D ( 'NONE', #8687, #3769, #1903 ) ;
#9192 = EDGE_CURVE ( 'NONE', #8921, #4065, #8732, .T. ) ;
#9193 =( BOUNDED_SURFACE ( )  B_SPLINE_SURFACE ( 3, 2, ( 
 ( #4201, #7009, #8987 ),
 ( #9046, #2385, #8113 ),
 ( #4139, #9104, #3455 ),
 ( #7258, #11819, #7129 ),
 ( #393, #6321, #10927 ),
 ( #3262, #6197, #1460 ),
 ( #10106, #7069, #520 ),
 ( #3329, #10866, #11938 ),
 ( #6261, #10804, #1582 ),
 ( #4260, #2328, #9865 ),
 ( #6135, #11879, #5267 ),
 ( #9925, #9989, #1397 ),
 ( #3207, #580, #4379 ),
 ( #5387, #2267, #5206 ),
 ( #4318, #8925, #3393 ),
 ( #455, #7191, #10994 ),
 ( #6074, #8053, #11059 ),
 ( #2455, #10049, #1524 ),
 ( #8178, #2521, #12000 ),
 ( #333, #7930, #11754 ),
 ( #1339, #5147, #1646 ),
 ( #10171, #7443, #7322 ),
 ( #2637, #10420, #6510 ),
 ( #1709, #5518, #9294 ),
 ( #12306, #715, #6625 ),
 ( #1766, #11310, #9231 ) ),
 .UNSPECIFIED., .F., .F., .F. ) 
 B_SPLINE_SURFACE_WITH_KNOTS ( ( 4, 2, 2, 2, 2, 2, 2, 2, 2, 2, 2, 2, 4 ),
 ( 3, 3 ),
 ( 0.006382978049045527277, 0.008387885753076827766, 0.009390339605092477143, 0.01039279345710812652, 0.01239770116113942701, 0.01340015501315507812, 0.01440260886517072750, 0.01540506271718637861, 0.01640751656920202972, 0.01841242427323332848, 0.01941487812524897785, 0.02041733197726462723, 0.02242223968129592598 ),
 ( 0.000000000000000000, 1.000000000000000000 ),
 .UNSPECIFIED. ) 
 GEOMETRIC_REPRESENTATION_ITEM ( )  RATIONAL_B_SPLINE_SURFACE ( (
 ( 1.000000000000000000, 0.8291561975888499525, 1.000000000000000000),
 ( 1.000000000000000000, 0.8291533992853559187, 1.000000000000000000),
 ( 1.000000000000000000, 0.8281244206746621872, 1.000000000000000000),
 ( 1.000000000000000000, 0.8251351734919457614, 1.000000000000000000),
 ( 1.000000000000000000, 0.8238971056969668361, 1.000000000000000000),
 ( 1.000000000000000000, 0.8209398665854361621, 1.000000000000000000),
 ( 1.000000000000000000, 0.8192278287709440221, 1.000000000000000000),
 ( 1.000000000000000000, 0.8135208904818045372, 1.000000000000000000),
 ( 1.000000000000000000, 0.8089311958808242942, 1.000000000000000000),
 ( 1.000000000000000000, 0.8010155071010776062, 1.000000000000000000),
 ( 1.000000000000000000, 0.7981992791122975994, 1.000000000000000000),
 ( 1.000000000000000000, 0.7923673440970770976, 1.000000000000000000),
 ( 1.000000000000000000, 0.7893380284541040570, 1.000000000000000000),
 ( 1.000000000000000000, 0.7830853791992800073, 1.000000000000000000),
 ( 1.000000000000000000, 0.7798619748040830357, 1.000000000000000000),
 ( 1.000000000000000000, 0.7732488416061537029, 1.000000000000000000),
 ( 1.000000000000000000, 0.7698413672833309684, 1.000000000000000000),
 ( 1.000000000000000000, 0.7595660318242437592, 1.000000000000000000),
 ( 1.000000000000000000, 0.7526475626048493295, 1.000000000000000000),
 ( 1.000000000000000000, 0.7423381171274799906, 1.000000000000000000),
 ( 1.000000000000000000, 0.7389127554685368526, 1.000000000000000000),
 ( 1.000000000000000000, 0.7321112719851028405, 1.000000000000000000),
 ( 1.000000000000000000, 0.7287565628962664466, 1.000000000000000000),
 ( 1.000000000000000000, 0.7189979416187094463, 1.000000000000000000),
 ( 1.000000000000000000, 0.7128432726192635016, 1.000000000000000000),
 ( 1.000000000000000000, 0.7071067811865476838, 1.000000000000000000) ) ) 
 REPRESENTATION_ITEM ( '' )  SURFACE ( )  );
#9194 = LINE ( 'NONE', #3659, #6010 ) ;
#9195 = VERTEX_POINT ( 'NONE', #6877 ) ;
#9196 = FACE_OUTER_BOUND ( 'NONE', #11621, .T. ) ;
#9197 = EDGE_CURVE ( 'NONE', #5363, #2747, #1829, .T. ) ;
#9198 = CARTESIAN_POINT ( 'NONE',  ( -32.15778161310143446, 87.00000000000000000, -8.660254037844435260 ) ) ;
#9199 = VERTEX_POINT ( 'NONE', #1951 ) ;
#9200 = AXIS2_PLACEMENT_3D ( 'NONE', #4860, #172, #2171 ) ;
#9201 = CARTESIAN_POINT ( 'NONE',  ( 7.594472908538985045, 34.78349364905407270, 79.50000000000000000 ) ) ;
#9202 = PLANE ( 'NONE',  #4980 ) ;
#9203 = ORIENTED_EDGE ( 'NONE', *, *, #9457, .T. ) ;
#9204 = CARTESIAN_POINT ( 'NONE',  ( -0.9407811293052825707, 17.00000000000008882, 79.50000000000000000 ) ) ;
#9205 = EDGE_CURVE ( 'NONE', #6384, #9696, #5763, .T. ) ;
#9206 = EDGE_CURVE ( 'NONE', #9781, #7928, #1326, .T. ) ;
#9207 = CIRCLE ( 'NONE', #9009, 0.2000000000000000944 ) ;
#9208 = ORIENTED_EDGE ( 'NONE', *, *, #89, .F. ) ;
#9209 = ORIENTED_EDGE ( 'NONE', *, *, #11053, .T. ) ;
#9210 = DIRECTION ( 'NONE',  ( -0.000000000000000000, -1.000000000000000000, -0.000000000000000000 ) ) ;
#9211 = CARTESIAN_POINT ( 'NONE',  ( -1.190781129305471087, 30.00000000000008882, 75.00000000000001421 ) ) ;
#9212 = ORIENTED_EDGE ( 'NONE', *, *, #11763, .F. ) ;
#9213 = DIRECTION ( 'NONE',  ( 0.000000000000000000, 1.000000000000000000, 0.000000000000000000 ) ) ;
#9214 = CARTESIAN_POINT ( 'NONE',  ( -28.12254474901590484, 87.93978760833334718, -10.28801392380147206 ) ) ;
#9215 = ORIENTED_EDGE ( 'NONE', *, *, #9281, .T. ) ;
#9216 = FACE_OUTER_BOUND ( 'NONE', #10664, .T. ) ;
#9217 = DIRECTION ( 'NONE',  ( 0.000000000000000000, 0.000000000000000000, 1.000000000000000000 ) ) ;
#9218 = CARTESIAN_POINT ( 'NONE',  ( -1.440781129305471087, 43.00000000000008527, 79.50000000000000000 ) ) ;
#9219 = AXIS2_PLACEMENT_3D ( 'NONE', #4273, #728, #11130 ) ;
#9220 = VECTOR ( 'NONE', #1938, 1000.000000000000114 ) ;
#9221 = EDGE_LOOP ( 'NONE', ( #12297, #954, #6988, #11939 ) ) ;
#9222 = CARTESIAN_POINT ( 'NONE',  ( 1.224646799147353533E-14, 260.0000000000000000, -100.0000000000000284 ) ) ;
#9223 = CARTESIAN_POINT ( 'NONE',  ( 9.942549119892305498, 36.71650635094628967, 80.00000000000000000 ) ) ;
#9224 = ORIENTED_EDGE ( 'NONE', *, *, #1079, .T. ) ;
#9225 = DIRECTION ( 'NONE',  ( 0.000000000000000000, 1.000000000000000000, 0.000000000000000000 ) ) ;
#9226 = LINE ( 'NONE', #711, #7264 ) ;
#9227 = VECTOR ( 'NONE', #4629, 999.9999999999998863 ) ;
#9228 = VERTEX_POINT ( 'NONE', #7057 ) ;
#9229 = AXIS2_PLACEMENT_3D ( 'NONE', #3789, #5850, #11401 ) ;
#9230 = DIRECTION ( 'NONE',  ( 0.000000000000000000, 1.000000000000000000, 0.000000000000000000 ) ) ;
#9231 = CARTESIAN_POINT ( 'NONE',  ( 77.45966692414835109, 45.00000000000009237, 20.00000000000000711 ) ) ;
#9232 = ORIENTED_EDGE ( 'NONE', *, *, #5402, .F. ) ;
#9233 = CARTESIAN_POINT ( 'NONE',  ( 149.1421356237320026, 17.07106781186555722, -24.99999999999998934 ) ) ;
#9234 = EDGE_CURVE ( 'NONE', #1251, #9416, #11927, .T. ) ;
#9235 = PLANE ( 'NONE',  #11297 ) ;
#9236 = CARTESIAN_POINT ( 'NONE',  ( 2.708734125000000326, 113.3749999986344079, 1.121994411437819084 ) ) ;
#9237 = CARTESIAN_POINT ( 'NONE',  ( 3.250000000000000444, 114.8749999972688158, 0.000000000000000000 ) ) ;
#9238 = EDGE_CURVE ( 'NONE', #3744, #7474, #2129, .T. ) ;
#9239 = AXIS2_PLACEMENT_3D ( 'NONE', #2120, #11351, #11413 ) ;
#9240 = ORIENTED_EDGE ( 'NONE', *, *, #6953, .F. ) ;
#9241 =( LENGTH_UNIT ( ) NAMED_UNIT ( * ) SI_UNIT ( .MILLI., .METRE. ) );
#9242 = VECTOR ( 'NONE', #6809, 1000.000000000000000 ) ;
#9243 = DIRECTION ( 'NONE',  ( -0.000000000000000000, 1.000000000000000000, -0.000000000000000000 ) ) ;
#9244 = CARTESIAN_POINT ( 'NONE',  ( 13.80921887069452758, 30.00000000000008882, 78.00000000000000000 ) ) ;
#9245 = CARTESIAN_POINT ( 'NONE',  ( 0.000000000000000000, 75.00000000000001421, 90.00000000000002842 ) ) ;
#9246 = VECTOR ( 'NONE', #1476, 1000.000000000000000 ) ;
#9247 = CARTESIAN_POINT ( 'NONE',  ( 4.025725221640849227, 21.46474596215575659, 79.50000000000000000 ) ) ;
#9248 = CIRCLE ( 'NONE', #7044, 90.00000000000002842 ) ;
#9249 = CARTESIAN_POINT ( 'NONE',  ( -32.13993895771326947, 87.28197645339797361, -8.497454856569977011 ) ) ;
#9250 = CARTESIAN_POINT ( 'NONE',  ( -16.19078112930547064, 30.00000000000008882, 73.23154106273422315 ) ) ;
#9251 = ADVANCED_FACE ( 'NONE', ( #321 ), #7118, .T. ) ;
#9252 = CARTESIAN_POINT ( 'NONE',  ( 13.63461413510340670, 27.67039418665449446, 73.75028910564438434 ) ) ;
#9253 = ORIENTED_EDGE ( 'NONE', *, *, #4267, .F. ) ;
#9254 = CARTESIAN_POINT ( 'NONE',  ( 2.298097038856278918, 111.8750000000000000, -2.298097038856279806 ) ) ;
#9255 = CYLINDRICAL_SURFACE ( 'NONE', #11158, 115.0000000000000284 ) ;
#9256 = CIRCLE ( 'NONE', #1911, 115.0000000000000284 ) ;
#9257 = CLOSED_SHELL ( 'NONE', ( #2257, #1446, #12021, #1358, #1988, #4076, #1121, #729, #10056, #4964, #4446, #10380, #3966, #8922, #1681, #7006, #253, #7749, #2214, #1125, #10166, #12046, #7642, #4937, #6103, #1105, #9117, #8168, #5110, #5704, #3920, #2037, #8495, #4526, #4295, #3358, #8814, #2334, #6230, #5821, #3833, #1973, #6849, #5446, #9715, #1711, #8520, #1987, #4845, #5287, #10821, #12034, #92, #12224, #9581, #8460, #6080, #8238, #527, #9745, #3860, #2036 ) ) ;
#9258 = DIRECTION ( 'NONE',  ( -0.000000000000000000, -1.000000000000000000, -0.000000000000000000 ) ) ;
#9259 = VECTOR ( 'NONE', #8952, 1000.000000000000000 ) ;
#9260 = ORIENTED_EDGE ( 'NONE', *, *, #4016, .F. ) ;
#9261 = DIRECTION ( 'NONE',  ( 0.000000000000000000, 1.000000000000000000, 0.000000000000000000 ) ) ;
#9262 = CARTESIAN_POINT ( 'NONE',  ( -73.35315233757310693, 19.78571428571397917, -34.26986240689829089 ) ) ;
#9263 = CARTESIAN_POINT ( 'NONE',  ( 74.58021194344081550, 17.74117554919819284, -24.47298709600785571 ) ) ;
#9264 = ORIENTED_EDGE ( 'NONE', *, *, #9888, .F. ) ;
#9265 = CIRCLE ( 'NONE', #3910, 28.00000000000000355 ) ;
#9266 = CARTESIAN_POINT ( 'NONE',  ( -25.00000000000000000, 345.0000000000000568, -29.99999999999999289 ) ) ;
#9267 = LINE ( 'NONE', #2792, #3978 ) ;
#9268 = EDGE_CURVE ( 'NONE', #10198, #2842, #1264, .T. ) ;
#9269 = VERTEX_POINT ( 'NONE', #11867 ) ;
#9270 = CARTESIAN_POINT ( 'NONE',  ( -24.76446302067273209, 275.0000000000000000, -102.0378428393002679 ) ) ;
#9271 =( BOUNDED_SURFACE ( )  B_SPLINE_SURFACE ( 3, 2, ( 
 ( #8258, #10187, #8192 ),
 ( #6274, #1661, #10121 ),
 ( #601, #8131, #4396 ),
 ( #9185, #5466, #9249 ) ),
 .UNSPECIFIED., .F., .F., .F. ) 
 B_SPLINE_SURFACE_WITH_KNOTS ( ( 4, 4 ),
 ( 3, 3 ),
 ( 0.08252307147639272034, 0.08572545668793904450 ),
 ( 0.000000000000000000, 1.000000000000000000 ),
 .UNSPECIFIED. ) 
 GEOMETRIC_REPRESENTATION_ITEM ( )  RATIONAL_B_SPLINE_SURFACE ( (
 ( 1.000000000000000000, 0.8237544710479142163, 1.000000000000000000),
 ( 1.000000000000000000, 0.8337078205039564205, 1.000000000000000000),
 ( 1.000000000000000000, 0.8426243553970728106, 1.000000000000000000),
 ( 1.000000000000000000, 0.8507194741069450394, 1.000000000000000000) ) ) 
 REPRESENTATION_ITEM ( '' )  SURFACE ( )  );
#9272 = ORIENTED_EDGE ( 'NONE', *, *, #4176, .F. ) ;
#9273 = DIRECTION ( 'NONE',  ( 0.000000000000000000, 0.000000000000000000, 1.000000000000000000 ) ) ;
#9275 = ORIENTED_EDGE ( 'NONE', *, *, #9234, .T. ) ;
#9274 = CARTESIAN_POINT ( 'NONE',  ( -8.500000000000000000, 165.5000000000000000, -7.483314773547880883 ) ) ;
#9276 = EDGE_LOOP ( 'NONE', ( #10937, #445, #312, #1707, #10659, #5166, #11887 ) ) ;
#9277 = DIRECTION ( 'NONE',  ( 0.000000000000000000, 1.000000000000000000, 0.000000000000000000 ) ) ;
#9278 = CARTESIAN_POINT ( 'NONE',  ( -25.00000000000000000, 570.2996408614167194, -29.99999999999999289 ) ) ;
#9279 = ORIENTED_EDGE ( 'NONE', *, *, #9053, .F. ) ;
#9280 = ADVANCED_FACE ( 'NONE', ( #7863 ), #4186, .F. ) ;
#9281 = EDGE_CURVE ( 'NONE', #4428, #9777, #8741, .T. ) ;
#9282 = SHAPE_REPRESENTATION_RELATIONSHIP ( 'NONE' , 'NONE' ,  #12244, #11672 ) ;
#9283 = DIRECTION ( 'NONE',  ( 0.000000000000000000, 0.000000000000000000, -1.000000000000000000 ) ) ;
#9284 = DIRECTION ( 'NONE',  ( 0.000000000000000000, -1.000000000000000000, 0.000000000000000000 ) ) ;
#9285 = PLANE ( 'NONE',  #5614 ) ;
#9286 = ORIENTED_EDGE ( 'NONE', *, *, #2595, .F. ) ;
#9287 = CARTESIAN_POINT ( 'NONE',  ( -4.975863863883684959E-16, 114.3124999986344079, -2.708734124999999882 ) ) ;
#9288 = DIRECTION ( 'NONE',  ( -0.000000000000000000, -1.000000000000000000, -0.000000000000000000 ) ) ;
#9289 = ORIENTED_EDGE ( 'NONE', *, *, #953, .F. ) ;
#9290 = DIRECTION ( 'NONE',  ( -0.000000000000000000, -0.4999999999999974465, 0.8660254037844401509 ) ) ;
#9291 = CARTESIAN_POINT ( 'NONE',  ( 72.61843774138907293, 50.00000000000000000, 18.75000000000000000 ) ) ;
#9292 = ORIENTED_EDGE ( 'NONE', *, *, #4621, .T. ) ;
#9293 = DIRECTION ( 'NONE',  ( 0.000000000000000000, 0.000000000000000000, 1.000000000000000000 ) ) ;
#9294 = CARTESIAN_POINT ( 'NONE',  ( 77.11786746747833377, 44.96870739097081326, 20.64504863446540384 ) ) ;
#9295 = ORIENTED_EDGE ( 'NONE', *, *, #2819, .F. ) ;
#9296 = LINE ( 'NONE', #783, #8879 ) ;
#9297 = LINE ( 'NONE', #4756, #8161 ) ;
#9298 = CARTESIAN_POINT ( 'NONE',  ( -1.915364268218908927, 111.9374999986344079, 1.915364268218909150 ) ) ;
#9299 = DIRECTION ( 'NONE',  ( 0.000000000000000000, 1.000000000000000000, 0.000000000000000000 ) ) ;
#9300 = EDGE_LOOP ( 'NONE', ( #1445, #2235, #9426, #10856 ) ) ;
#9301 = ORIENTED_EDGE ( 'NONE', *, *, #8751, .F. ) ;
#9302 =( NAMED_UNIT ( * ) SI_UNIT ( $, .STERADIAN. ) SOLID_ANGLE_UNIT ( ) );
#9303 = VECTOR ( 'NONE', #4300, 1000.000000000000000 ) ;
#9304 = EDGE_CURVE ( 'NONE', #10742, #8153, #4517, .T. ) ;
#9305 = EDGE_CURVE ( 'NONE', #3388, #9777, #4245, .T. ) ;
#9306 = CYLINDRICAL_SURFACE ( 'NONE', #2262, 95.00000000000002842 ) ;
#9307 = DIRECTION ( 'NONE',  ( 0.000000000000000000, 1.000000000000000000, 0.000000000000000000 ) ) ;
#9309 = EDGE_CURVE ( 'NONE', #9087, #4827, #11682, .T. ) ;
#9308 = CARTESIAN_POINT ( 'NONE',  ( -30.14540500433760783, 76.99999999999997158, 4.927060346216586950 ) ) ;
#9310 = CARTESIAN_POINT ( 'NONE',  ( -11.19078112930532853, 29.75000000000005684, 79.50000000000000000 ) ) ;
#9311 = CARTESIAN_POINT ( 'NONE',  ( -27.55156151032566214, 86.54395234961377525, -11.88489976664090442 ) ) ;
#9312 = CARTESIAN_POINT ( 'NONE',  ( -15.76722741620018731, 33.57691821622091766, 73.32398149152362521 ) ) ;
#9313 = CIRCLE ( 'NONE', #158, 2.055000000000000160 ) ;
#9314 = DIRECTION ( 'NONE',  ( 0.000000000000000000, 0.000000000000000000, -1.000000000000000000 ) ) ;
#9315 = CARTESIAN_POINT ( 'NONE',  ( -2.298097038856279806, 113.6250000000000000, -2.298097038856279362 ) ) ;
#9316 = DIRECTION ( 'NONE',  ( -0.4999999999999985012, 0.8660254037844394848, 0.000000000000000000 ) ) ;
#9317 = AXIS2_PLACEMENT_3D ( 'NONE', #694, #8346, #4495 ) ;
#9318 = DIRECTION ( 'NONE',  ( 0.4999999999999878431, -0.8660254037844455910, 0.000000000000000000 ) ) ;
#9319 = EDGE_LOOP ( 'NONE', ( #11540, #4754, #8211, #3424 ) ) ;
#9320 = DIRECTION ( 'NONE',  ( 0.8660254037844385966, -0.5000000000000000000, 0.000000000000000000 ) ) ;
#9321 = PLANE ( 'NONE',  #2282 ) ;
#9322 = CARTESIAN_POINT ( 'NONE',  ( 70.79098555864042908, 20.00000000000008882, -24.99999999999999645 ) ) ;
#9323 = VERTEX_POINT ( 'NONE', #2252 ) ;
#9324 = FACE_OUTER_BOUND ( 'NONE', #11379, .T. ) ;
#9325 = DIRECTION ( 'NONE',  ( 6.938893903907222067E-15, 1.000000000000000000, 0.000000000000000000 ) ) ;
#9326 = VECTOR ( 'NONE', #11637, 1000.000000000000000 ) ;
#9327 = ORIENTED_EDGE ( 'NONE', *, *, #8858, .T. ) ;
#9328 = CARTESIAN_POINT ( 'NONE',  ( -25.00000000000000000, 345.0000000000000568, -29.99999999999999289 ) ) ;
#9329 = ORIENTED_EDGE ( 'NONE', *, *, #12329, .F. ) ;
#9330 = EDGE_CURVE ( 'NONE', #8931, #7224, #7610, .T. ) ;
#9331 = DIRECTION ( 'NONE',  ( 0.000000000000000000, 0.000000000000000000, 1.000000000000000000 ) ) ;
#9332 = VECTOR ( 'NONE', #8089, 1000.000000000000000 ) ;
#9334 = ORIENTED_EDGE ( 'NONE', *, *, #3285, .T. ) ;
#9333 = CARTESIAN_POINT ( 'NONE',  ( -14.19078112930532853, 30.25000000000008882, 80.00000000000000000 ) ) ;
#9335 = ORIENTED_EDGE ( 'NONE', *, *, #6315, .F. ) ;
#9336 = EDGE_CURVE ( 'NONE', #1834, #7484, #10880, .T. ) ;
#9337 = DIRECTION ( 'NONE',  ( -0.8660254037844424824, -0.4999999999999933387, 0.000000000000000000 ) ) ;
#9338 = EDGE_LOOP ( 'NONE', ( #4687, #9240, #925, #4604, #10852 ) ) ;
#9339 = LINE ( 'NONE', #1868, #3896 ) ;
#9340 = DIRECTION ( 'NONE',  ( -0.9682458365518540333, -4.961309141293670183E-14, -0.2500000000000003331 ) ) ;
#9341 = PLANE ( 'NONE',  #5407 ) ;
#9342 = ORIENTED_EDGE ( 'NONE', *, *, #2759, .F. ) ;
#9343 = CARTESIAN_POINT ( 'NONE',  ( -2.708734124999999882, 114.0624999986344079, 3.317242575922456639E-16 ) ) ;
#9344 = CARTESIAN_POINT ( 'NONE',  ( 69.52686081652184669, 20.00000000000009237, 28.12500000000000000 ) ) ;
#9345 = AXIS2_PLACEMENT_3D ( 'NONE', #11047, #7248, #11111 ) ;
#9346 = EDGE_CURVE ( 'NONE', #8931, #9024, #5869, .T. ) ;
#9347 = ORIENTED_EDGE ( 'NONE', *, *, #1655, .T. ) ;
#9348 = EDGE_CURVE ( 'NONE', #3011, #7492, #260, .T. ) ;
#9349 = CARTESIAN_POINT ( 'NONE',  ( 4.025725221640669815, 38.53525403784453118, 79.50000000000000000 ) ) ;
#9350 = CARTESIAN_POINT ( 'NONE',  ( 69.76162866618027181, 43.49853569900138694, 27.53780242413599666 ) ) ;
#9351 = ORIENTED_EDGE ( 'NONE', *, *, #12134, .F. ) ;
#9352 = CARTESIAN_POINT ( 'NONE',  ( -25.00000000000000000, 345.0000000000000568, -59.99999999999999289 ) ) ;
#9353 = DIRECTION ( 'NONE',  ( -0.000000000000000000, -1.000000000000000000, -0.000000000000000000 ) ) ;
#9354 = ORIENTED_EDGE ( 'NONE', *, *, #5598, .T. ) ;
#9355 = VECTOR ( 'NONE', #5109, 1000.000000000000000 ) ;
#9356 = VECTOR ( 'NONE', #10439, 1000.000000000000114 ) ;
#9357 = CARTESIAN_POINT ( 'NONE',  ( -25.00000000000000000, 445.0000000000000568, -90.00000000000000000 ) ) ;
#9358 = DIRECTION ( 'NONE',  ( 0.000000000000000000, 0.000000000000000000, 1.000000000000000000 ) ) ;
#9359 = CARTESIAN_POINT ( 'NONE',  ( -1.915364268218908927, 113.9374999986344079, 1.915364268218909150 ) ) ;
#9360 = LINE ( 'NONE', #6281, #9454 ) ;
#9361 = ORIENTED_EDGE ( 'NONE', *, *, #11212, .T. ) ;
#9362 = ORIENTED_EDGE ( 'NONE', *, *, #937, .F. ) ;
#9363 = SHAPE_REPRESENTATION_RELATIONSHIP ( 'NONE' , 'NONE' ,  #10952, #11228 ) ;
#9364 = CIRCLE ( 'NONE', #612, 73.00000000000002842 ) ;
#9365 = CIRCLE ( 'NONE', #10369, 15.00000000000000000 ) ;
#9366 = ADVANCED_FACE ( 'NONE', ( #11044 ), #11107, .T. ) ;
#9367 = EDGE_CURVE ( 'NONE', #9534, #2576, #1754, .T. ) ;
#9368 = SURFACE_SIDE_STYLE ('',( #3834 ) ) ;
#9369 = CARTESIAN_POINT ( 'NONE',  ( 5.200000000000002842, 0.000000000000000000, 0.000000000000000000 ) ) ;
#9370 = ORIENTED_EDGE ( 'NONE', *, *, #10146, .F. ) ;
#9371 = DIRECTION ( 'NONE',  ( -0.000000000000000000, -0.000000000000000000, -1.000000000000000000 ) ) ;
#9372 = CARTESIAN_POINT ( 'NONE',  ( 116.4243635975512490, 275.0000000000000000, 45.50129185973946733 ) ) ;
#9373 = VECTOR ( 'NONE', #4993, 1000.000000000000000 ) ;
#9374 = CARTESIAN_POINT ( 'NONE',  ( -15.13490964629960978, 35.55200036032155708, 73.45732584901404039 ) ) ;
#9375 = FACE_OUTER_BOUND ( 'NONE', #6357, .T. ) ;
#9376 = CARTESIAN_POINT ( 'NONE',  ( 11.80921887069467324, 29.75000000000018474, 79.50000000000000000 ) ) ;
#9377 = AXIS2_PLACEMENT_3D ( 'NONE', #1109, #3036, #6839 ) ;
#9378 = AXIS2_PLACEMENT_3D ( 'NONE', #12022, #12210, #3477 ) ;
#9379 = CARTESIAN_POINT ( 'NONE',  ( 0.000000000000000000, 65.00000000000000000, 0.000000000000000000 ) ) ;
#9380 = PLANE ( 'NONE',  #1898 ) ;
#9381 = VERTEX_POINT ( 'NONE', #1634 ) ;
#9382 = DIRECTION ( 'NONE',  ( 1.000000000000000000, 0.000000000000000000, 0.000000000000000000 ) ) ;
#9383 = DIRECTION ( 'NONE',  ( 0.000000000000000000, 0.000000000000000000, -1.000000000000000000 ) ) ;
#9384 = DIRECTION ( 'NONE',  ( 0.000000000000000000, 1.000000000000000000, 0.000000000000000000 ) ) ;
#9385 = VERTEX_POINT ( 'NONE', #7369 ) ;
#9386 = CARTESIAN_POINT ( 'NONE',  ( 3.061616997868383043E-15, 75.00000000000001421, -25.00000000000000000 ) ) ;
#9387 = ADVANCED_FACE ( 'NONE', ( #569 ), #9886, .T. ) ;
#9388 = DIRECTION ( 'NONE',  ( 0.000000000000000000, 1.000000000000000000, 0.000000000000000000 ) ) ;
#9389 = TOROIDAL_SURFACE ( 'NONE', #4030, 105.0000000000000284, 5.000000000000000000 ) ;
#9390 = VERTEX_POINT ( 'NONE', #8225 ) ;
#9391 = FACE_OUTER_BOUND ( 'NONE', #7434, .T. ) ;
#9392 = ORIENTED_EDGE ( 'NONE', *, *, #9023, .T. ) ;
#9393 = AXIS2_PLACEMENT_3D ( 'NONE', #12041, #8905, #9085 ) ;
#9394 = DIRECTION ( 'NONE',  ( 0.000000000000000000, 0.000000000000000000, 1.000000000000000000 ) ) ;
#9395 = CARTESIAN_POINT ( 'NONE',  ( 4.163799117101000559E-16, 115.0000000000000000, -3.399999999999999911 ) ) ;
#9396 = VERTEX_POINT ( 'NONE', #11170 ) ;
#9397 = DIRECTION ( 'NONE',  ( 0.000000000000000000, 0.000000000000000000, 1.000000000000000000 ) ) ;
#9398 = ORIENTED_EDGE ( 'NONE', *, *, #6788, .F. ) ;
#9399 = CARTESIAN_POINT ( 'NONE',  ( 0.000000000000000000, 0.000000000000000000, 0.000000000000000000 ) ) ;
#9400 = CARTESIAN_POINT ( 'NONE',  ( 9.450654096908945471E-15, 44.95265997413478942, 75.00000000000001421 ) ) ;
#9401 = FACE_OUTER_BOUND ( 'NONE', #2347, .T. ) ;
#9402 = CARTESIAN_POINT ( 'NONE',  ( 0.000000000000000000, 87.00000000000000000, 0.000000000000000000 ) ) ;
#9403 = ORIENTED_EDGE ( 'NONE', *, *, #6863, .F. ) ;
#9404 = CARTESIAN_POINT ( 'NONE',  ( -1.915364268218909594, 112.1874999986344079, -1.915364268218908927 ) ) ;
#9405 = CIRCLE ( 'NONE', #9612, 28.00000000000000355 ) ;
#9406 = EDGE_CURVE ( 'NONE', #11096, #4895, #4431, .T. ) ;
#9407 = FACE_OUTER_BOUND ( 'NONE', #10153, .T. ) ;
#9408 = ADVANCED_FACE ( 'NONE', ( #2626 ), #698, .T. ) ;
#9409 = ORIENTED_EDGE ( 'NONE', *, *, #11893, .F. ) ;
#9410 = CARTESIAN_POINT ( 'NONE',  ( 0.000000000000000000, 153.0000000000000000, 0.000000000000000000 ) ) ;
#9411 = CARTESIAN_POINT ( 'NONE',  ( 72.28493664348427217, 49.93201633561922392, 20.00732221823095713 ) ) ;
#9412 = VERTEX_POINT ( 'NONE', #8162 ) ;
#9413 = CARTESIAN_POINT ( 'NONE',  ( 2.500000000000000000, 2.357898499370431722, -2.818925648462311528E-15 ) ) ;
#9414 = CARTESIAN_POINT ( 'NONE',  ( 5.525725221640672480, 41.13333024919784719, 80.00000000000000000 ) ) ;
#9415 = VECTOR ( 'NONE', #4275, 1000.000000000000114 ) ;
#9416 = VERTEX_POINT ( 'NONE', #8411 ) ;
#9417 = CARTESIAN_POINT ( 'NONE',  ( -25.00000000000000000, 570.2996408614167194, -59.99999999999999289 ) ) ;
#9418 = LINE ( 'NONE', #11435, #9561 ) ;
#9419 = CARTESIAN_POINT ( 'NONE',  ( 1.915364268218908705, 111.4374999986344079, -1.915364268218909594 ) ) ;
#9420 = EDGE_CURVE ( 'NONE', #11122, #7224, #12097, .T. ) ;
#9421 = EDGE_CURVE ( 'NONE', #1550, #1153, #11504, .T. ) ;
#9422 = FACE_OUTER_BOUND ( 'NONE', #5459, .T. ) ;
#9423 = VERTEX_POINT ( 'NONE', #11234 ) ;
#9424 = VECTOR ( 'NONE', #8742, 1000.000000000000000 ) ;
#9425 = AXIS2_PLACEMENT_3D ( 'NONE', #9065, #7889, #9002 ) ;
#9426 = ORIENTED_EDGE ( 'NONE', *, *, #8769, .T. ) ;
#9427 = DIRECTION ( 'NONE',  ( 0.000000000000000000, -0.000000000000000000, 1.000000000000000000 ) ) ;
#9428 = ORIENTED_EDGE ( 'NONE', *, *, #249, .T. ) ;
#9429 = LINE ( 'NONE', #5774, #2236 ) ;
#9430 = DIRECTION ( 'NONE',  ( -0.000000000000000000, 1.000000000000000000, -0.000000000000000000 ) ) ;
#9431 = FACE_OUTER_BOUND ( 'NONE', #1810, .T. ) ;
#9432 = LINE ( 'NONE', #3841, #11994 ) ;
#9433 = EDGE_CURVE ( 'NONE', #4433, #5644, #11990, .T. ) ;
#9434 = EDGE_CURVE ( 'NONE', #11226, #3370, #1434, .T. ) ;
#9435 = AXIS2_PLACEMENT_3D ( 'NONE', #4439, #7253, #10103 ) ;
#9436 = CARTESIAN_POINT ( 'NONE',  ( 0.000000000000000000, 275.0000000000000000, 0.000000000000000000 ) ) ;
#9437 = EDGE_CURVE ( 'NONE', #12186, #5470, #7984, .T. ) ;
#9438 = AXIS2_PLACEMENT_3D ( 'NONE', #6108, #488, #5172 ) ;
#9439 = CARTESIAN_POINT ( 'NONE',  ( 69.72804008650257401, 43.29323253992120613, -27.62368211345594204 ) ) ;
#9440 = CIRCLE ( 'NONE', #10244, 2.041999999999999815 ) ;
#9441 = DIRECTION ( 'NONE',  ( -1.000000000000000000, 0.000000000000000000, 0.000000000000000000 ) ) ;
#9442 = VERTEX_POINT ( 'NONE', #3624 ) ;
#9443 = PRODUCT_RELATED_PRODUCT_CATEGORY ( 'part', '', ( #9761 ) ) ;
#9444 = CARTESIAN_POINT ( 'NONE',  ( 5.000000000000000888, 4.250000000000000000, 0.000000000000000000 ) ) ;
#9445 = LINE ( 'NONE', #1045, #3093 ) ;
#9446 = CARTESIAN_POINT ( 'NONE',  ( 70.96239324365633649, 17.73867115851379950, -24.49110472308180064 ) ) ;
#9447 = VERTEX_POINT ( 'NONE', #3563 ) ;
#9448 =( GEOMETRIC_REPRESENTATION_CONTEXT ( 3 ) GLOBAL_UNCERTAINTY_ASSIGNED_CONTEXT ( ( #11888 ) ) GLOBAL_UNIT_ASSIGNED_CONTEXT ( ( #9501, #7646, #4844 ) ) REPRESENTATION_CONTEXT ( 'NONE', 'WORKASPACE' ) );
#9449 = PRODUCT_DEFINITION_SHAPE ( 'NONE', 'NONE',  #12355 ) ;
#9450 = CARTESIAN_POINT ( 'NONE',  ( -1.190781129305471087, 30.00000000000008882, 80.00000000000000000 ) ) ;
#9451 = VECTOR ( 'NONE', #11269, 1000.000000000000000 ) ;
#9452 = ORIENTED_EDGE ( 'NONE', *, *, #10991, .T. ) ;
#9453 = PLANE ( 'NONE',  #1000 ) ;
#9454 = VECTOR ( 'NONE', #12311, 1000.000000000000000 ) ;
#9455 = EDGE_CURVE ( 'NONE', #1744, #5680, #2032, .T. ) ;
#9456 = ORIENTED_EDGE ( 'NONE', *, *, #7342, .F. ) ;
#9457 = EDGE_CURVE ( 'NONE', #5052, #8595, #3027, .T. ) ;
#9458 = LINE ( 'NONE', #4859, #8708 ) ;
#9459 = FACE_OUTER_BOUND ( 'NONE', #2853, .T. ) ;
#9460 = ORIENTED_EDGE ( 'NONE', *, *, #7083, .F. ) ;
#9461 = VECTOR ( 'NONE', #9555, 1000.000000000000000 ) ;
#9462 = CARTESIAN_POINT ( 'NONE',  ( 0.2500000000000002220, 0.000000000000000000, 4.250000000000000000 ) ) ;
#9463 = DIRECTION ( 'NONE',  ( -1.000000000000000000, 0.000000000000000000, 0.000000000000000000 ) ) ;
#9464 = ORIENTED_EDGE ( 'NONE', *, *, #3782, .T. ) ;
#9465 = ADVANCED_FACE ( 'NONE', ( #4617 ), #7432, .F. ) ;
#9466 = CARTESIAN_POINT ( 'NONE',  ( 2.500000000000000000, -2.357898499370432166, 3.035766082959412415E-15 ) ) ;
#9467 = CIRCLE ( 'NONE', #11677, 110.0000000000000284 ) ;
#9468 = CARTESIAN_POINT ( 'NONE',  ( 0.000000000000000000, -10.00000000000000000, 0.000000000000000000 ) ) ;
#9469 = DIRECTION ( 'NONE',  ( 0.000000000000000000, -1.000000000000000000, 0.000000000000000000 ) ) ;
#9470 = ORIENTED_EDGE ( 'NONE', *, *, #8545, .F. ) ;
#9471 = CARTESIAN_POINT ( 'NONE',  ( -1.121994411437818862, 110.6249999986343937, 2.708734125000000326 ) ) ;
#9472 = CARTESIAN_POINT ( 'NONE',  ( -12.57411137850301763, 23.71650635094618664, 79.50000000000000000 ) ) ;
#9473 = STYLED_ITEM ( 'NONE', ( #2964 ), #8720 ) ;
#9474 = VERTEX_POINT ( 'NONE', #7178 ) ;
#9475 = CARTESIAN_POINT ( 'NONE',  ( 10.19254911989230727, 36.28349364905406560, 79.50000000000000000 ) ) ;
#9476 = FACE_OUTER_BOUND ( 'NONE', #8345, .T. ) ;
#9477 = ORIENTED_EDGE ( 'NONE', *, *, #6484, .T. ) ;
#9478 = DIRECTION ( 'NONE',  ( -0.000000000000000000, 1.000000000000000000, -0.000000000000000000 ) ) ;
#9479 = FACE_OUTER_BOUND ( 'NONE', #8724, .T. ) ;
#9480 = ORIENTED_EDGE ( 'NONE', *, *, #6024, .F. ) ;
#9481 = DIRECTION ( 'NONE',  ( -0.000000000000000000, -1.000000000000000000, -0.000000000000000000 ) ) ;
#9482 = CARTESIAN_POINT ( 'NONE',  ( 11.80921887069467324, 29.75000000000018474, 79.50000000000000000 ) ) ;
#9483 = CARTESIAN_POINT ( 'NONE',  ( 138.5355339059338462, 63.53553390593273775, -20.00000000000000000 ) ) ;
#9484 = AXIS2_PLACEMENT_3D ( 'NONE', #8912, #9724, #6182 ) ;
#9485 = LINE ( 'NONE', #3354, #2504 ) ;
#9486 = ORIENTED_EDGE ( 'NONE', *, *, #11242, .F. ) ;
#9487 = ORIENTED_EDGE ( 'NONE', *, *, #9457, .F. ) ;
#9488 = CARTESIAN_POINT ( 'NONE',  ( -1.190781129305471087, 30.00000000000008882, 80.00000000000000000 ) ) ;
#9489 = CARTESIAN_POINT ( 'NONE',  ( 0.000000000000000000, -5.000000000000000000, 0.000000000000000000 ) ) ;
#9490 = VERTEX_POINT ( 'NONE', #1572 ) ;
#9491 = ADVANCED_FACE ( 'NONE', ( #6247 ), #7608, .F. ) ;
#9492 = DIRECTION ( 'NONE',  ( 0.000000000000000000, 1.000000000000000000, 0.000000000000000000 ) ) ;
#9493 = CARTESIAN_POINT ( 'NONE',  ( 0.000000000000000000, 285.0000000000000568, 0.000000000000000000 ) ) ;
#9494 = LINE ( 'NONE', #10503, #3312 ) ;
#9495 = CYLINDRICAL_SURFACE ( 'NONE', #1238, 25.00000000000000000 ) ;
#9496 = ORIENTED_EDGE ( 'NONE', *, *, #2787, .T. ) ;
#9497 = PRODUCT_DEFINITION_CONTEXT ( 'detailed design', #557, 'design' ) ;
#9498 = EDGE_CURVE ( 'NONE', #3728, #357, #3934, .T. ) ;
#9499 = EDGE_CURVE ( 'NONE', #592, #4639, #6211, .T. ) ;
#9500 = CARTESIAN_POINT ( 'NONE',  ( 74.16198487097054226, 40.16707677251596209, -25.00000000000000000 ) ) ;
#9501 =( LENGTH_UNIT ( ) NAMED_UNIT ( * ) SI_UNIT ( .MILLI., .METRE. ) );
#9502 = EDGE_LOOP ( 'NONE', ( #1525, #8830, #4227, #5435 ) ) ;
#9503 = VECTOR ( 'NONE', #8646, 1000.000000000000000 ) ;
#9504 = CARTESIAN_POINT ( 'NONE',  ( 0.000000000000000000, 65.00000000000000000, 0.000000000000000000 ) ) ;
#9505 = DIRECTION ( 'NONE',  ( 0.000000000000000000, 0.000000000000000000, 1.000000000000000000 ) ) ;
#9506 = CARTESIAN_POINT ( 'NONE',  ( 0.000000000000000000, 122.5000000000000000, 0.000000000000000000 ) ) ;
#9507 = CARTESIAN_POINT ( 'NONE',  ( 70.03362437693311904, 14.90552201415263767, -26.84082993662185501 ) ) ;
#9508 = ORIENTED_EDGE ( 'NONE', *, *, #3384, .T. ) ;
#9509 = DIRECTION ( 'NONE',  ( 0.8660254037844434816, 0.4999999999999913958, 0.000000000000000000 ) ) ;
#9510 = CARTESIAN_POINT ( 'NONE',  ( 0.000000000000000000, 170.0000000000000000, 0.000000000000000000 ) ) ;
#9511 = ORIENTED_EDGE ( 'NONE', *, *, #1454, .T. ) ;
#9512 = DIRECTION ( 'NONE',  ( 0.000000000000000000, 0.000000000000000000, 1.000000000000000000 ) ) ;
#9513 = EDGE_CURVE ( 'NONE', #4699, #6802, #5806, .T. ) ;
#9514 = AXIS2_PLACEMENT_3D ( 'NONE', #4875, #5689, #7795 ) ;
#9515 = EDGE_CURVE ( 'NONE', #5710, #10706, #6613, .T. ) ;
#9516 = ORIENTED_EDGE ( 'NONE', *, *, #10096, .F. ) ;
#9517 = FACE_OUTER_BOUND ( 'NONE', #9548, .T. ) ;
#9518 = LINE ( 'NONE', #7841, #4641 ) ;
#9519 = ORIENTED_EDGE ( 'NONE', *, *, #6256, .F. ) ;
#9520 = CARTESIAN_POINT ( 'NONE',  ( -3.250000000000000444, 111.3749999972688158, 3.980102097228898231E-16 ) ) ;
#9521 = DIRECTION ( 'NONE',  ( 0.000000000000000000, 0.000000000000000000, 1.000000000000000000 ) ) ;
#9522 = ORIENTED_EDGE ( 'NONE', *, *, #6837, .F. ) ;
#9523 = SHAPE_DEFINITION_REPRESENTATION ( #8557, #778 ) ;
#9524 = CARTESIAN_POINT ( 'NONE',  ( 73.35315233757310693, 79.55366347814538130, -0.2371791482635408899 ) ) ;
#9525 = DIRECTION ( 'NONE',  ( -0.000000000000000000, -1.000000000000000000, -0.000000000000000000 ) ) ;
#9526 = DIRECTION ( 'NONE',  ( -0.000000000000000000, -0.000000000000000000, 1.000000000000000000 ) ) ;
#9527 = EDGE_LOOP ( 'NONE', ( #5803, #8150, #7652, #10057 ) ) ;
#9528 = CARTESIAN_POINT ( 'NONE',  ( 2.708734124999999882, 111.6249999986344079, 1.121994411437818862 ) ) ;
#9529 = ADVANCED_FACE ( 'NONE', ( #8917 ), #1065, .T. ) ;
#9530 = ADVANCED_FACE ( 'NONE', ( #2868, #9401 ), #10343, .T. ) ;
#9531 = CARTESIAN_POINT ( 'NONE',  ( -1.346194077712560944, 113.5624999972688300, -3.249999999999999556 ) ) ;
#9532 = AXIS2_PLACEMENT_3D ( 'NONE', #2111, #10459, #4723 ) ;
#9533 = AXIS2_PLACEMENT_3D ( 'NONE', #7378, #3514, #6318 ) ;
#9534 = VERTEX_POINT ( 'NONE', #1813 ) ;
#9535 = LINE ( 'NONE', #1375, #10131 ) ;
#9536 = CARTESIAN_POINT ( 'NONE',  ( -1.190781129305471087, 30.00000000000008882, 80.00000000000000000 ) ) ;
#9537 = ORIENTED_EDGE ( 'NONE', *, *, #5190, .F. ) ;
#9538 = CARTESIAN_POINT ( 'NONE',  ( 1.990051048614449116E-16, 110.2500000000000000, 3.250000000000000444 ) ) ;
#9539 = CARTESIAN_POINT ( 'NONE',  ( -20.00000000000000000, 63.00000000000000000, -67.08203932499371547 ) ) ;
#9540 = ORIENTED_EDGE ( 'NONE', *, *, #11573, .F. ) ;
#9541 = LINE ( 'NONE', #4821, #9623 ) ;
#9542 = CARTESIAN_POINT ( 'NONE',  ( 20.00000000000000355, 7.965803112215716020, 57.08203932499370836 ) ) ;
#9543 = CARTESIAN_POINT ( 'NONE',  ( 0.000000000000000000, 285.0000000000000568, 0.000000000000000000 ) ) ;
#9544 = VECTOR ( 'NONE', #572, 1000.000000000000000 ) ;
#9545 = CARTESIAN_POINT ( 'NONE',  ( 2.708734124999999437, 114.4999999986344079, -1.121994411437820638 ) ) ;
#9546 = CARTESIAN_POINT ( 'NONE',  ( 2.298097038856278918, 112.8750000000000000, -2.298097038856279806 ) ) ;
#9547 = EDGE_CURVE ( 'NONE', #9228, #9696, #6674, .T. ) ;
#9548 = EDGE_LOOP ( 'NONE', ( #5358, #9279, #11861, #4760, #2383 ) ) ;
#9549 = VECTOR ( 'NONE', #8614, 1000.000000000000000 ) ;
#9550 = ORIENTED_EDGE ( 'NONE', *, *, #1516, .F. ) ;
#9551 = AXIS2_PLACEMENT_3D ( 'NONE', #11207, #7280, #6406 ) ;
#9552 = CIRCLE ( 'NONE', #2005, 2.500000000000000444 ) ;
#9553 = PRODUCT_DEFINITION_SHAPE ( 'NONE', 'NONE',  #5201 ) ;
#9554 = FACE_OUTER_BOUND ( 'NONE', #768, .T. ) ;
#9555 = DIRECTION ( 'NONE',  ( -0.000000000000000000, 1.000000000000000000, -0.000000000000000000 ) ) ;
#9556 = ORIENTED_EDGE ( 'NONE', *, *, #2050, .F. ) ;
#9557 = DIRECTION ( 'NONE',  ( -1.000000000000000000, 0.000000000000000000, 0.000000000000000000 ) ) ;
#9558 = CARTESIAN_POINT ( 'NONE',  ( 0.000000000000000000, 340.0000000000000000, 105.0000000000000284 ) ) ;
#9559 = CARTESIAN_POINT ( 'NONE',  ( -6.000000000000000000, 65.00000000000000000, 69.74238309665079782 ) ) ;
#9560 = CARTESIAN_POINT ( 'NONE',  ( 2.979367062500000163, 114.1562499993171969, 0.000000000000000000 ) ) ;
#9561 = VECTOR ( 'NONE', #4515, 1000.000000000000000 ) ;
#9562 = CARTESIAN_POINT ( 'NONE',  ( 0.000000000000000000, 0.000000000000000000, 0.000000000000000000 ) ) ;
#9563 = ADVANCED_FACE ( 'NONE', ( #10477 ), #948, .F. ) ;
#9564 = EDGE_CURVE ( 'NONE', #544, #8739, #119, .T. ) ;
#9565 = VECTOR ( 'NONE', #11586, 1000.000000000000000 ) ;
#9566 = CARTESIAN_POINT ( 'NONE',  ( 75.13748311126856549, 43.33995240362821733, -23.73500236559034704 ) ) ;
#9567 = CARTESIAN_POINT ( 'NONE',  ( 135.0000000000011084, 67.07106781186550393, -19.99999999999999645 ) ) ;
#9568 = AXIS2_PLACEMENT_3D ( 'NONE', #2810, #6614, #3809 ) ;
#9569 = CARTESIAN_POINT ( 'NONE',  ( 29.42287733398170602, 85.62135522733748871, 10.27237124600371487 ) ) ;
#9570 = DIRECTION ( 'NONE',  ( 0.000000000000000000, -0.4999999999999976130, 0.8660254037844400399 ) ) ;
#9571 = CARTESIAN_POINT ( 'NONE',  ( 3.250000000000000444, 113.0000000000000000, 0.000000000000000000 ) ) ;
#9572 = CARTESIAN_POINT ( 'NONE',  ( 76.84714931290172046, 15.12440032299506143, -21.12007276954078350 ) ) ;
#9573 = VERTEX_POINT ( 'NONE', #7546 ) ;
#9574 = CARTESIAN_POINT ( 'NONE',  ( -32.18413411689675030, 86.41755723128771649, -8.996527527148016290 ) ) ;
#9575 = CARTESIAN_POINT ( 'NONE',  ( -7.690781129305409358, 41.25833024919774772, 80.00000000000000000 ) ) ;
#9576 = VECTOR ( 'NONE', #8998, 1000.000000000000114 ) ;
#9577 = EDGE_LOOP ( 'NONE', ( #8893, #4326, #4180, #9984 ) ) ;
#9578 = DIRECTION ( 'NONE',  ( 0.000000000000000000, 0.000000000000000000, 1.000000000000000000 ) ) ;
#9579 = AXIS2_PLACEMENT_3D ( 'NONE', #5503, #9284, #765 ) ;
#9580 = EDGE_CURVE ( 'NONE', #10794, #9030, #883, .T. ) ;
#9581 = ADVANCED_FACE ( 'NONE', ( #8593 ), #1869, .T. ) ;
#9582 = ORIENTED_EDGE ( 'NONE', *, *, #7217, .F. ) ;
#9583 = LINE ( 'NONE', #11347, #11320 ) ;
#9584 = CARTESIAN_POINT ( 'NONE',  ( 1.347111479062088996E-14, 290.0000000000000568, 110.0000000000000284 ) ) ;
#9585 = ORIENTED_EDGE ( 'NONE', *, *, #7316, .T. ) ;
#9586 = CARTESIAN_POINT ( 'NONE',  ( 89.80805993797383735, 285.0000000000000568, 81.82974571984303225 ) ) ;
#9587 = CARTESIAN_POINT ( 'NONE',  ( -16.19078112930547064, 30.00000000000008882, 75.00000000000001421 ) ) ;
#9588 = VERTEX_POINT ( 'NONE', #3869 ) ;
#9589 = DIRECTION ( 'NONE',  ( 0.000000000000000000, 0.000000000000000000, 1.000000000000000000 ) ) ;
#9590 = CARTESIAN_POINT ( 'NONE',  ( -75.98513253586240523, 275.0000000000000000, 72.46557550663233371 ) ) ;
#9591 = CARTESIAN_POINT ( 'NONE',  ( 5.092712519748452848, 41.38333024919784719, 79.50000000000000000 ) ) ;
#9592 = EDGE_CURVE ( 'NONE', #11360, #7682, #10986, .T. ) ;
#9593 = EDGE_CURVE ( 'NONE', #10035, #9024, #7799, .T. ) ;
#9594 = EDGE_LOOP ( 'NONE', ( #9486, #4440, #779, #8248, #2357 ) ) ;
#9595 = CARTESIAN_POINT ( 'NONE',  ( -4.975863863883684959E-16, 114.0624999986344079, -2.708734125000000326 ) ) ;
#9596 = CARTESIAN_POINT ( 'NONE',  ( -3.250000000000000444, 113.3124999972688016, 1.346194077712559389 ) ) ;
#9597 = VECTOR ( 'NONE', #5149, 1000.000000000000000 ) ;
#9598 = ORIENTED_EDGE ( 'NONE', *, *, #277, .F. ) ;
#9599 = DIRECTION ( 'NONE',  ( -1.000000000000000000, 0.000000000000000000, -6.938893903907229610E-17 ) ) ;
#9600 = CARTESIAN_POINT ( 'NONE',  ( 75.00000000000001421, 20.00000000000009237, -19.99999999999999645 ) ) ;
#9601 = ORIENTED_EDGE ( 'NONE', *, *, #10274, .T. ) ;
#9602 = DIRECTION ( 'NONE',  ( 0.000000000000000000, 0.000000000000000000, -1.000000000000000000 ) ) ;
#9603 = CARTESIAN_POINT ( 'NONE',  ( 69.90350624952220926, 15.60330682347095710, 27.17578603812306426 ) ) ;
#9604 = ORIENTED_EDGE ( 'NONE', *, *, #9798, .F. ) ;
#9605 = DIRECTION ( 'NONE',  ( 0.000000000000000000, 0.000000000000000000, -1.000000000000000000 ) ) ;
#9606 = DIRECTION ( 'NONE',  ( 1.000000000000000000, -1.040834085586083310E-14, 0.000000000000000000 ) ) ;
#9607 = DIRECTION ( 'NONE',  ( -1.000000000000000000, 0.000000000000000000, -0.000000000000000000 ) ) ;
#9608 = AXIS2_PLACEMENT_3D ( 'NONE', #8647, #1930, #3862 ) ;
#9609 = CARTESIAN_POINT ( 'NONE',  ( -4.975863863883684959E-16, 114.3124999986344079, -2.708734124999999882 ) ) ;
#9610 = CARTESIAN_POINT ( 'NONE',  ( 77.45966692414835109, 15.00000000000008882, 20.00000000000000355 ) ) ;
#9611 = ORIENTED_EDGE ( 'NONE', *, *, #3757, .T. ) ;
#9612 = AXIS2_PLACEMENT_3D ( 'NONE', #1670, #5480, #2783 ) ;
#9613 = LINE ( 'NONE', #392, #7452 ) ;
#9614 = EDGE_CURVE ( 'NONE', #12345, #10879, #7204, .T. ) ;
#9615 = DIRECTION ( 'NONE',  ( -0.5000000000000005551, -0.8660254037844382635, 0.000000000000000000 ) ) ;
#9616 = ORIENTED_EDGE ( 'NONE', *, *, #3877, .T. ) ;
#9617 = CARTESIAN_POINT ( 'NONE',  ( 142.0710678118665555, 59.99999999999998579, -20.00000000000000000 ) ) ;
#9618 = DIRECTION ( 'NONE',  ( 0.000000000000000000, 0.000000000000000000, 1.000000000000000000 ) ) ;
#9619 = DIRECTION ( 'NONE',  ( 1.564230817409691233E-15, 0.000000000000000000, -1.000000000000000000 ) ) ;
#9620 = ADVANCED_FACE ( 'NONE', ( #11209 ), #7345, .T. ) ;
#9621 = ORIENTED_EDGE ( 'NONE', *, *, #4468, .T. ) ;
#9622 = CIRCLE ( 'NONE', #5263, 72.00000000000002842 ) ;
#9623 = VECTOR ( 'NONE', #8610, 1000.000000000000000 ) ;
#9624 = SURFACE_STYLE_USAGE ( .BOTH. , #12327 ) ;
#9625 = ORIENTED_EDGE ( 'NONE', *, *, #2062, .T. ) ;
#9626 = CARTESIAN_POINT ( 'NONE',  ( 71.69575657208368114, 49.37823943430655049, -22.01828877003865514 ) ) ;
#9627 = CARTESIAN_POINT ( 'NONE',  ( -29.63582346253862454, 77.00000000000000000, 4.660254037844413944 ) ) ;
#9628 = AXIS2_PLACEMENT_3D ( 'NONE', #8790, #10669, #9720 ) ;
#9629 = DIRECTION ( 'NONE',  ( -0.000000000000000000, 1.000000000000000000, -0.000000000000000000 ) ) ;
#9630 = VECTOR ( 'NONE', #10699, 1000.000000000000000 ) ;
#9631 = LINE ( 'NONE', #1110, #93 ) ;
#9632 = CYLINDRICAL_SURFACE ( 'NONE', #9858, 10.00000000000000178 ) ;
#9633 = ORIENTED_EDGE ( 'NONE', *, *, #6942, .T. ) ;
#9634 = CARTESIAN_POINT ( 'NONE',  ( 0.2500000000000002220, 0.000000000000000000, 0.000000000000000000 ) ) ;
#9635 = DIRECTION ( 'NONE',  ( 1.000000000000000000, 0.000000000000000000, 0.000000000000000000 ) ) ;
#9636 = ORIENTED_EDGE ( 'NONE', *, *, #6836, .F. ) ;
#9637 = FACE_OUTER_BOUND ( 'NONE', #8540, .T. ) ;
#9638 = VECTOR ( 'NONE', #5053, 1000.000000000000000 ) ;
#9639 = AXIS2_PLACEMENT_3D ( 'NONE', #11493, #3005, #1258 ) ;
#9640 = VERTEX_POINT ( 'NONE', #2659 ) ;
#9641 = DIRECTION ( 'NONE',  ( -0.8660254037844398178, -0.4999999999999977796, 0.000000000000000000 ) ) ;
#9642 = CARTESIAN_POINT ( 'NONE',  ( 76.59271415824169082, 44.76269180811209480, 21.55336028430496143 ) ) ;
#9643 = ORIENTED_EDGE ( 'NONE', *, *, #9809, .F. ) ;
#9644 = CARTESIAN_POINT ( 'NONE',  ( 31.33267436902169933, 77.00000000000000000, -7.087639215986555108 ) ) ;
#9645 = CARTESIAN_POINT ( 'NONE',  ( -25.00000000000000000, 445.0000000000000568, -95.00000000000000000 ) ) ;
#9646 = ORIENTED_EDGE ( 'NONE', *, *, #124, .T. ) ;
#9647 = EDGE_CURVE ( 'NONE', #9199, #1231, #6470, .T. ) ;
#9648 = DIRECTION ( 'NONE',  ( 0.000000000000000000, 0.000000000000000000, 1.000000000000000000 ) ) ;
#9649 =( GEOMETRIC_REPRESENTATION_CONTEXT ( 3 ) GLOBAL_UNCERTAINTY_ASSIGNED_CONTEXT ( ( #7139 ) ) GLOBAL_UNIT_ASSIGNED_CONTEXT ( ( #2285, #3097, #6961 ) ) REPRESENTATION_CONTEXT ( 'NONE', 'WORKASPACE' ) );
#9650 = DIRECTION ( 'NONE',  ( 1.000000000000000000, 0.000000000000000000, 0.000000000000000000 ) ) ;
#9651 = DIRECTION ( 'NONE',  ( 0.000000000000000000, 1.000000000000000000, 0.000000000000000000 ) ) ;
#9652 = EDGE_LOOP ( 'NONE', ( #2673, #7976, #7583, #1789 ) ) ;
#9653 = CARTESIAN_POINT ( 'NONE',  ( -2.708734125000000326, 111.8124999986344079, 3.317242575922457132E-16 ) ) ;
#9654 = CARTESIAN_POINT ( 'NONE',  ( -3.250000000000001776, 112.4374999972688300, -1.346194077712558723 ) ) ;
#9655 = CIRCLE ( 'NONE', #4100, 100.0000000000000284 ) ;
#9656 = EDGE_LOOP ( 'NONE', ( #3374, #8489, #8001, #11716 ) ) ;
#9657 = EDGE_CURVE ( 'NONE', #4316, #7882, #6663, .T. ) ;
#9658 = LINE ( 'NONE', #9475, #1389 ) ;
#9659 = EDGE_CURVE ( 'NONE', #9755, #4568, #4578, .T. ) ;
#9660 = CARTESIAN_POINT ( 'NONE',  ( 145.0000000000011369, 225.0000000000000853, -20.00000000000000000 ) ) ;
#9661 = EDGE_LOOP ( 'NONE', ( #7041, #644, #7752, #615 ) ) ;
#9662 = CIRCLE ( 'NONE', #8266, 4.999999999999997335 ) ;
#9663 = CARTESIAN_POINT ( 'NONE',  ( -9.726035167149685634, 24.78349364905394125, 79.50000000000000000 ) ) ;
#9664 = DIRECTION ( 'NONE',  ( 0.4999999999999877875, -0.8660254037844457020, 0.000000000000000000 ) ) ;
#9665 = VERTEX_POINT ( 'NONE', #8200 ) ;
#9666 = FACE_OUTER_BOUND ( 'NONE', #6250, .T. ) ;
#9667 = FACE_OUTER_BOUND ( 'NONE', #1636, .T. ) ;
#9668 = DIRECTION ( 'NONE',  ( 0.000000000000000000, 0.000000000000000000, -1.000000000000000000 ) ) ;
#9669 = DIRECTION ( 'NONE',  ( 0.000000000000000000, 1.000000000000000000, 0.000000000000000000 ) ) ;
#9670 = DIRECTION ( 'NONE',  ( 0.000000000000000000, 0.000000000000000000, -1.000000000000000000 ) ) ;
#9671 = CARTESIAN_POINT ( 'NONE',  ( -4.975863863883684959E-16, 113.3124999986344079, -2.708734124999999882 ) ) ;
#9672 = AXIS2_PLACEMENT_3D ( 'NONE', #4707, #8381, #12204 ) ;
#9673 = EDGE_CURVE ( 'NONE', #7589, #6190, #9194, .T. ) ;
#9674 = SHAPE_REPRESENTATION ( 'Die-Cast Base Motor Housing', ( #1612 ), #10763 ) ;
#9675 = ORIENTED_EDGE ( 'NONE', *, *, #8649, .T. ) ;
#9676 = CARTESIAN_POINT ( 'NONE',  ( 75.00000000000001421, 15.00000000000008882, 25.00000000000000000 ) ) ;
#9677 = DIRECTION ( 'NONE',  ( 0.000000000000000000, -0.000000000000000000, 1.000000000000000000 ) ) ;
#9678 = EDGE_LOOP ( 'NONE', ( #12215, #6036, #5215, #8458 ) ) ;
#9679 = LINE ( 'NONE', #10373, #10601 ) ;
#9680 = LINE ( 'NONE', #3026, #8363 ) ;
#9681 = CIRCLE ( 'NONE', #7700, 75.00000000000001421 ) ;
#9682 = CARTESIAN_POINT ( 'NONE',  ( 30.00100000000000122, 77.00000000000000000, 8.660254037844445918 ) ) ;
#9683 = CARTESIAN_POINT ( 'NONE',  ( 2.708734124999999882, 111.2499999986344079, -1.121994411437820416 ) ) ;
#9684 = EDGE_LOOP ( 'NONE', ( #401, #3499, #315, #11909, #5118 ) ) ;
#9685 = FILL_AREA_STYLE ('',( #155 ) ) ;
#9686 = EDGE_CURVE ( 'NONE', #2386, #7815, #8386, .T. ) ;
#9687 = ORIENTED_EDGE ( 'NONE', *, *, #3487, .F. ) ;
#9688 = EDGE_CURVE ( 'NONE', #7164, #7492, #4406, .T. ) ;
#9689 = ADVANCED_FACE ( 'NONE', ( #12270 ), #10073, .T. ) ;
#9690 =( NAMED_UNIT ( * ) PLANE_ANGLE_UNIT ( ) SI_UNIT ( $, .RADIAN. ) );
#9691 = CARTESIAN_POINT ( 'NONE',  ( 0.000000000000000000, 50.00000000000000000, 0.000000000000000000 ) ) ;
#9692 = DIRECTION ( 'NONE',  ( 1.000000000000000000, -7.011174048739587977E-15, 0.000000000000000000 ) ) ;
#9693 = ORIENTED_EDGE ( 'NONE', *, *, #5125, .F. ) ;
#9694 = CARTESIAN_POINT ( 'NONE',  ( 0.000000000000000000, 265.0000000000000000, -15.00000000000000000 ) ) ;
#9695 = CARTESIAN_POINT ( 'NONE',  ( 72.32585155008061406, 14.83851532874689738, -19.87486525338129795 ) ) ;
#9696 = VERTEX_POINT ( 'NONE', #8387 ) ;
#9697 = DIRECTION ( 'NONE',  ( -4.440892098500626162E-15, 0.000000000000000000, 1.000000000000000000 ) ) ;
#9698 = CARTESIAN_POINT ( 'NONE',  ( 165.0000000000011369, 225.0000000000000853, -25.00000000000000000 ) ) ;
#9699 = ORIENTED_EDGE ( 'NONE', *, *, #7521, .F. ) ;
#9700 = CYLINDRICAL_SURFACE ( 'NONE', #3594, 10.49999999999999822 ) ;
#9701 = AXIS2_PLACEMENT_3D ( 'NONE', #12164, #3493, #11224 ) ;
#9702 = ORIENTED_EDGE ( 'NONE', *, *, #5216, .F. ) ;
#9703 = CARTESIAN_POINT ( 'NONE',  ( 1.224646799147353375E-14, 260.0000000000000000, 100.0000000000000142 ) ) ;
#9704 = CARTESIAN_POINT ( 'NONE',  ( -18.80690714323172941, 275.0000000000000000, -123.5771024247852665 ) ) ;
#9705 = ORIENTED_EDGE ( 'NONE', *, *, #7166, .F. ) ;
#9706 = CARTESIAN_POINT ( 'NONE',  ( 6.000000000000000000, 65.00000000000000000, 69.74238309665078361 ) ) ;
#9707 = FACE_BOUND ( 'NONE', #8970, .T. ) ;
#9708 = VERTEX_POINT ( 'NONE', #6285 ) ;
#9709 = DIRECTION ( 'NONE',  ( 1.000000000000000000, 0.000000000000000000, 0.000000000000000000 ) ) ;
#9710 = CARTESIAN_POINT ( 'NONE',  ( 20.00000000000000000, 50.00000000000000000, 67.08203932499371547 ) ) ;
#9711 = ORIENTED_EDGE ( 'NONE', *, *, #10494, .F. ) ;
#9712 = CARTESIAN_POINT ( 'NONE',  ( 2.708734125000000326, 112.3749999986344221, 1.121994411437818862 ) ) ;
#9713 = CARTESIAN_POINT ( 'NONE',  ( -1.346194077712559389, 111.1874999972688016, 3.250000000000000444 ) ) ;
#9714 = EDGE_CURVE ( 'NONE', #8835, #5671, #5352, .T. ) ;
#9715 = ADVANCED_FACE ( 'NONE', ( #5417 ), #9129, .T. ) ;
#9716 = ORIENTED_EDGE ( 'NONE', *, *, #4410, .T. ) ;
#9717 = CARTESIAN_POINT ( 'NONE',  ( -7.474274778359198734, 41.38333024919781167, 79.50000000000000000 ) ) ;
#9718 = CARTESIAN_POINT ( 'NONE',  ( 0.000000000000000000, 40.00000000000009237, -25.00000000000000000 ) ) ;
#9719 = ORIENTED_EDGE ( 'NONE', *, *, #10254, .T. ) ;
#9720 = DIRECTION ( 'NONE',  ( 0.000000000000000000, 0.000000000000000000, -1.000000000000000000 ) ) ;
#9721 = CARTESIAN_POINT ( 'NONE',  ( 117.9289321881355193, 50.00000000000008527, -19.99999999999999645 ) ) ;
#9722 = VERTEX_POINT ( 'NONE', #7283 ) ;
#9723 = CARTESIAN_POINT ( 'NONE',  ( 0.000000000000000000, 92.00000000000000000, -30.00000000000000000 ) ) ;
#9724 = DIRECTION ( 'NONE',  ( -0.000000000000000000, -1.000000000000000000, -0.000000000000000000 ) ) ;
#9725 = CARTESIAN_POINT ( 'NONE',  ( 0.000000000000000000, 0.000000000000000000, 79.50000000000000000 ) ) ;
#9726 = VECTOR ( 'NONE', #6269, 1000.000000000000000 ) ;
#9727 = LINE ( 'NONE', #1207, #11352 ) ;
#9728 = DIRECTION ( 'NONE',  ( 0.000000000000000000, 0.000000000000000000, -1.000000000000000000 ) ) ;
#9729 = CARTESIAN_POINT ( 'NONE',  ( 1.915364268218909150, 111.6874999986344079, 1.915364268218909150 ) ) ;
#9730 = AXIS2_PLACEMENT_3D ( 'NONE', #2981, #2854, #3854 ) ;
#9731 = VECTOR ( 'NONE', #211, 1000.000000000000000 ) ;
#9732 = EDGE_CURVE ( 'NONE', #2354, #9722, #5471, .T. ) ;
#9733 = ORIENTED_EDGE ( 'NONE', *, *, #3034, .T. ) ;
#9734 = ORIENTED_EDGE ( 'NONE', *, *, #7040, .F. ) ;
#9735 = CARTESIAN_POINT ( 'NONE',  ( 170.0000000000011369, 35.00000000000006395, 22.92893218813452449 ) ) ;
#9736 = CARTESIAN_POINT ( 'NONE',  ( 13.80921887069452758, 30.92976843375813445, 73.71774192269630532 ) ) ;
#9737 = VERTEX_POINT ( 'NONE', #3535 ) ;
#9738 = DIRECTION ( 'NONE',  ( 1.000000000000000000, 0.000000000000000000, 6.938893903907228378E-17 ) ) ;
#9739 = AXIS2_PLACEMENT_3D ( 'NONE', #2320, #11992, #1637 ) ;
#9740 = PLANE ( 'NONE',  #5197 ) ;
#9741 = CARTESIAN_POINT ( 'NONE',  ( -12.40744471183567299, 36.57216878364999246, 80.00000000000000000 ) ) ;
#9742 = PRESENTATION_LAYER_ASSIGNMENT (  '', '', ( #5976 ) ) ;
#9743 = DIRECTION ( 'NONE',  ( 0.000000000000000000, 0.000000000000000000, -1.000000000000000000 ) ) ;
#9744 = EDGE_CURVE ( 'NONE', #8617, #867, #11137, .T. ) ;
#9745 = ADVANCED_FACE ( 'NONE', ( #603 ), #1542, .T. ) ;
#9746 =( BOUNDED_CURVE ( )  B_SPLINE_CURVE ( 3, ( #534, #6148, #4330, #11950 ),
 .UNSPECIFIED., .F., .F. ) 
 B_SPLINE_CURVE_WITH_KNOTS ( ( 4, 4 ),
 ( 4.284962911267360397, 4.868362425771961099 ),
 .UNSPECIFIED. ) 
 CURVE ( )  GEOMETRIC_REPRESENTATION_ITEM ( )  RATIONAL_B_SPLINE_CURVE ( ( 1.000000000000000000, 0.9718376280744367435, 0.9718376280744367435, 1.000000000000000000 ) ) 
 REPRESENTATION_ITEM ( '' )  );
#9747 = ORIENTED_EDGE ( 'NONE', *, *, #3057, .F. ) ;
#9748 = CARTESIAN_POINT ( 'NONE',  ( 0.000000000000000000, 50.00000000000000000, -75.00000000000002842 ) ) ;
#9749 = VERTEX_POINT ( 'NONE', #3414 ) ;
#9750 = CIRCLE ( 'NONE', #4382, 2.700000000000000622 ) ;
#9751 = B_SPLINE_CURVE_WITH_KNOTS ( 'NONE', 3,
 ( #1823, #4564, #6441, #10230 ),
 .UNSPECIFIED., .F., .F.,
 ( 4, 4 ),
 ( 0.0009573067811869144170, 0.001207306781186545577 ),
 .UNSPECIFIED. ) ;
#9752 = LINE ( 'NONE', #2159, #3765 ) ;
#9753 = CARTESIAN_POINT ( 'NONE',  ( 30.50145854323926642, 85.38003226577610860, 9.854387615546505330 ) ) ;
#9754 = PLANE ( 'NONE',  #6209 ) ;
#9755 = VERTEX_POINT ( 'NONE', #6276 ) ;
#9756 = CARTESIAN_POINT ( 'NONE',  ( 2.500000000000000000, -2.629050547790028551E-15, -2.041999999999999815 ) ) ;
#9757 = DIRECTION ( 'NONE',  ( -0.8660254037844383745, 0.5000000000000006661, 0.000000000000000000 ) ) ;
#9758 = AXIS2_PLACEMENT_3D ( 'NONE', #3044, #4982, #9578 ) ;
#9759 = LINE ( 'NONE', #1480, #280 ) ;
#9760 = AXIS2_PLACEMENT_3D ( 'NONE', #4204, #7994, #4263 ) ;
#9761 = PRODUCT ( 'Die-Cast Base Motor Housing', 'Die-Cast Base Motor Housing', '', ( #2935 ) ) ;
#9762 = DIRECTION ( 'NONE',  ( 0.8660254037844410391, 0.4999999999999958367, -0.000000000000000000 ) ) ;
#9763 = ORIENTED_EDGE ( 'NONE', *, *, #3275, .T. ) ;
#9764 = CARTESIAN_POINT ( 'NONE',  ( -12.32411137850303184, 36.71650635094619730, 80.00000000000000000 ) ) ;
#9765 = AXIS2_PLACEMENT_3D ( 'NONE', #6675, #5927, #1940 ) ;
#9766 = EDGE_LOOP ( 'NONE', ( #10608, #1218, #1757, #1308, #1853 ) ) ;
#9767 = CARTESIAN_POINT ( 'NONE',  ( -11.19078112930532498, 30.25000000000005684, 80.00000000000000000 ) ) ;
#9768 = ORIENTED_EDGE ( 'NONE', *, *, #10770, .T. ) ;
#9769 = CARTESIAN_POINT ( 'NONE',  ( 34.80930551369991122, 75.84619333735180646, -7.994103450571739877 ) ) ;
#9770 = EDGE_CURVE ( 'NONE', #3822, #5348, #8779, .T. ) ;
#9771 = CARTESIAN_POINT ( 'NONE',  ( 27.57052686557079468, 86.63064495281062705, 11.84084938503489148 ) ) ;
#9772 = EDGE_LOOP ( 'NONE', ( #5333, #9470, #6541, #521 ) ) ;
#9773 = AXIS2_PLACEMENT_3D ( 'NONE', #1076, #7912, #10606 ) ;
#9774 = CYLINDRICAL_SURFACE ( 'NONE', #5264, 30.00000000000000711 ) ;
#9775 = VECTOR ( 'NONE', #3597, 1000.000000000000000 ) ;
#9776 = CARTESIAN_POINT ( 'NONE',  ( -7.474274778359196070, 18.61666975080236597, 80.00000000000000000 ) ) ;
#9777 = VERTEX_POINT ( 'NONE', #4335 ) ;
#9778 = CARTESIAN_POINT ( 'NONE',  ( -2.708734125000000770, 111.8749999986343937, -1.121994411437818639 ) ) ;
#9779 = CARTESIAN_POINT ( 'NONE',  ( 1.346194077712559389, 114.0624999972688016, 3.250000000000000444 ) ) ;
#9780 = CIRCLE ( 'NONE', #1211, 70.00000000000001421 ) ;
#9781 = VERTEX_POINT ( 'NONE', #10123 ) ;
#9782 = CARTESIAN_POINT ( 'NONE',  ( 27.67899820261485999, 88.38261385519929547, 11.05501148229834030 ) ) ;
#9783 = CARTESIAN_POINT ( 'NONE',  ( -3.619653695503104451, 15.18885885628891863, 74.91437445603884271 ) ) ;
#9784 = ORIENTED_EDGE ( 'NONE', *, *, #8397, .T. ) ;
#9785 = LINE ( 'NONE', #9663, #6598 ) ;
#9786 = CARTESIAN_POINT ( 'NONE',  ( -1.440781129305471087, 43.00000000000008527, 80.00000000000000000 ) ) ;
#9787 = EDGE_CURVE ( 'NONE', #9178, #3388, #3815, .T. ) ;
#9788 = VERTEX_POINT ( 'NONE', #7402 ) ;
#9789 = FACE_OUTER_BOUND ( 'NONE', #618, .T. ) ;
#9790 = CARTESIAN_POINT ( 'NONE',  ( 75.53289395085349156, 43.87018216231679446, -23.18166983250910818 ) ) ;
#9791 = LINE ( 'NONE', #322, #3795 ) ;
#9792 = EDGE_LOOP ( 'NONE', ( #1548, #5961 ) ) ;
#9793 = DIRECTION ( 'NONE',  ( 0.000000000000000000, 0.000000000000000000, -1.000000000000000000 ) ) ;
#9794 = EDGE_CURVE ( 'NONE', #1438, #8296, #2406, .T. ) ;
#9795 = AXIS2_PLACEMENT_3D ( 'NONE', #5741, #4381, #9463 ) ;
#9796 = CARTESIAN_POINT ( 'NONE',  ( 71.74671581198677472, 15.26885267741330132, 21.97107035890156013 ) ) ;
#9797 = ORIENTED_EDGE ( 'NONE', *, *, #10765, .T. ) ;
#9798 = EDGE_CURVE ( 'NONE', #6916, #12030, #11987, .T. ) ;
#9799 = DIRECTION ( 'NONE',  ( 0.000000000000000000, -0.000000000000000000, 1.000000000000000000 ) ) ;
#9800 = ORIENTED_EDGE ( 'NONE', *, *, #2441, .F. ) ;
#9801 = DIRECTION ( 'NONE',  ( 0.8660254037844377084, -0.5000000000000015543, 0.000000000000000000 ) ) ;
#9802 = LINE ( 'NONE', #5772, #9461 ) ;
#9803 = ORIENTED_EDGE ( 'NONE', *, *, #582, .T. ) ;
#9804 = CARTESIAN_POINT ( 'NONE',  ( 5.309218870694537351, 18.74166975080233044, 80.00000000000000000 ) ) ;
#9805 = FACE_OUTER_BOUND ( 'NONE', #5204, .T. ) ;
#9806 = CARTESIAN_POINT ( 'NONE',  ( 0.000000000000000000, 65.00000000000000000, 0.000000000000000000 ) ) ;
#9807 = DIRECTION ( 'NONE',  ( 0.000000000000000000, 0.000000000000000000, 1.000000000000000000 ) ) ;
#9808 = EDGE_CURVE ( 'NONE', #6417, #8096, #5409, .T. ) ;
#9809 = EDGE_CURVE ( 'NONE', #5368, #3755, #3350, .T. ) ;
#9810 = ORIENTED_EDGE ( 'NONE', *, *, #2019, .T. ) ;
#9811 = AXIS2_PLACEMENT_3D ( 'NONE', #3847, #10695, #8511 ) ;
#9812 = PRESENTATION_STYLE_ASSIGNMENT (( #6027 ) ) ;
#9813 = EDGE_CURVE ( 'NONE', #1550, #7936, #3592, .T. ) ;
#9814 = CARTESIAN_POINT ( 'NONE',  ( 1.836970198721029589E-15, 127.0000000000000000, 15.00000000000000000 ) ) ;
#9815 = DIRECTION ( 'NONE',  ( 0.000000000000000000, 0.000000000000000000, 1.000000000000000000 ) ) ;
#9816 = LINE ( 'NONE', #8071, #1504 ) ;
#9817 = CARTESIAN_POINT ( 'NONE',  ( 30.94187416189151918, 76.19472969970551901, -6.055023111780714729 ) ) ;
#9818 = MECHANICAL_DESIGN_GEOMETRIC_PRESENTATION_REPRESENTATION (  '', ( #1671 ), #11030 ) ;
#9819 = CIRCLE ( 'NONE', #6083, 15.00000000000000000 ) ;
#9820 = CARTESIAN_POINT ( 'NONE',  ( 71.93323519045088688, 10.35045604464705349, -21.22984507177766034 ) ) ;
#9821 = CARTESIAN_POINT ( 'NONE',  ( 2.708734125000000326, 113.3124999986344079, 0.000000000000000000 ) ) ;
#9822 = ORIENTED_EDGE ( 'NONE', *, *, #9420, .F. ) ;
#9823 = DIRECTION ( 'NONE',  ( -0.8660254037844399289, -0.4999999999999977796, 0.000000000000000000 ) ) ;
#9824 = AXIS2_PLACEMENT_3D ( 'NONE', #714, #5266, #9924 ) ;
#9825 = CIRCLE ( 'NONE', #8442, 9.999999999999998224 ) ;
#9826 = EDGE_LOOP ( 'NONE', ( #42, #5094 ) ) ;
#9827 = CARTESIAN_POINT ( 'NONE',  ( -12.32411137850302119, 23.28349364905396612, 79.50000000000000000 ) ) ;
#9828 = ORIENTED_EDGE ( 'NONE', *, *, #10354, .F. ) ;
#9829 = CARTESIAN_POINT ( 'NONE',  ( 4.163799117101000559E-16, 109.0000000000000000, -3.399999999999999911 ) ) ;
#9830 = CARTESIAN_POINT ( 'NONE',  ( 27.30089691780743877, 86.86968904112121947, 12.43627868308088935 ) ) ;
#9831 = VERTEX_POINT ( 'NONE', #7148 ) ;
#9832 = DIRECTION ( 'NONE',  ( 1.000000000000000000, 0.000000000000000000, 0.000000000000000000 ) ) ;
#9833 = CARTESIAN_POINT ( 'NONE',  ( -27.88763417807736289, 88.17431669512683357, -10.69423021798056084 ) ) ;
#9834 = VECTOR ( 'NONE', #2056, 1000.000000000000000 ) ;
#9835 = VERTEX_POINT ( 'NONE', #5343 ) ;
#9836 = CARTESIAN_POINT ( 'NONE',  ( -1.121994411437820416, 112.9999999986343937, -2.708734124999999882 ) ) ;
#9837 = CIRCLE ( 'NONE', #88, 105.0000000000000426 ) ;
#9838 = ADVANCED_FACE ( 'NONE', ( #10945 ), #11203, .F. ) ;
#9839 = EDGE_CURVE ( 'NONE', #6431, #11751, #7000, .T. ) ;
#9840 = ORIENTED_EDGE ( 'NONE', *, *, #2567, .F. ) ;
#9841 = CARTESIAN_POINT ( 'NONE',  ( 29.14112381217240255, 87.50172632198248834, 9.529269519012832035 ) ) ;
#9842 = EDGE_CURVE ( 'NONE', #1236, #3768, #10178, .T. ) ;
#9843 = CARTESIAN_POINT ( 'NONE',  ( 0.000000000000000000, 10.00000000000017586, 0.000000000000000000 ) ) ;
#9844 = CIRCLE ( 'NONE', #6082, 15.00000000000000000 ) ;
#9845 = ORIENTED_EDGE ( 'NONE', *, *, #800, .F. ) ;
#9846 = AXIS2_PLACEMENT_3D ( 'NONE', #8039, #3378, #10979 ) ;
#9847 = DIRECTION ( 'NONE',  ( -0.000000000000000000, 1.287488025362403787E-15, 1.000000000000000000 ) ) ;
#9848 = DIRECTION ( 'NONE',  ( 0.7071067811865495711, 0.7071067811865455743, -0.000000000000000000 ) ) ;
#9849 = ORIENTED_EDGE ( 'NONE', *, *, #10513, .T. ) ;
#9850 = CYLINDRICAL_SURFACE ( 'NONE', #6483, 73.00000000000002842 ) ;
#9851 = CARTESIAN_POINT ( 'NONE',  ( -29.75437749274565391, 83.76094350395922561, -7.050043618115805266 ) ) ;
#9852 = DIRECTION ( 'NONE',  ( -1.000000000000000000, -0.000000000000000000, -0.000000000000000000 ) ) ;
#9853 = VERTEX_POINT ( 'NONE', #1663 ) ;
#9854 = DIRECTION ( 'NONE',  ( 0.000000000000000000, 0.000000000000000000, -1.000000000000000000 ) ) ;
#9855 = CARTESIAN_POINT ( 'NONE',  ( 70.79098555865897424, 19.78735728330005372, 24.99999999997159961 ) ) ;
#9856 = VECTOR ( 'NONE', #3223, 1000.000000000000000 ) ;
#9857 = CLOSED_SHELL ( 'NONE', ( #9529, #10919, #481, #2657, #2364, #7762, #1181, #3718, #4022, #9099, #5970 ) ) ;
#9858 = AXIS2_PLACEMENT_3D ( 'NONE', #6031, #8072, #1541 ) ;
#9859 = ORIENTED_EDGE ( 'NONE', *, *, #2623, .F. ) ;
#9860 = PLANE ( 'NONE',  #6471 ) ;
#9861 = CARTESIAN_POINT ( 'NONE',  ( 75.73945001075168193, 44.09015450245603063, -22.88037593554885518 ) ) ;
#9862 = ORIENTED_EDGE ( 'NONE', *, *, #5867, .T. ) ;
#9863 = PRODUCT_DEFINITION_SHAPE ( 'NONE', 'NONE',  #12357 ) ;
#9864 = DIRECTION ( 'NONE',  ( -0.000000000000000000, -1.000000000000000000, -0.000000000000000000 ) ) ;
#9865 = CARTESIAN_POINT ( 'NONE',  ( 74.91301266955075278, 42.95546542084321118, 24.03638115574963052 ) ) ;
#9866 = ORIENTED_EDGE ( 'NONE', *, *, #7228, .T. ) ;
#9867 = FACE_OUTER_BOUND ( 'NONE', #2431, .T. ) ;
#9868 = VECTOR ( 'NONE', #5311, 999.9999999999998863 ) ;
#9869 = DIRECTION ( 'NONE',  ( -0.000000000000000000, 1.000000000000000000, -0.000000000000000000 ) ) ;
#9870 = DIRECTION ( 'NONE',  ( -0.2358520287683116834, 0.000000000000000000, 0.9717889794219068955 ) ) ;
#9871 = DIRECTION ( 'NONE',  ( -0.000000000000000000, -1.000000000000000000, -0.000000000000000000 ) ) ;
#9872 = CONICAL_SURFACE ( 'NONE', #942, 3.399999999999999911, 1.029744258676658974 ) ;
#9873 = EDGE_CURVE ( 'NONE', #5952, #12219, #11791, .T. ) ;
#9874 = ORIENTED_EDGE ( 'NONE', *, *, #2583, .T. ) ;
#9875 = EDGE_LOOP ( 'NONE', ( #8271, #1320, #6495, #9633, #1505 ) ) ;
#9876 = ADVANCED_FACE ( 'NONE', ( #11328 ), #1728, .T. ) ;
#9877 = AXIS2_PLACEMENT_3D ( 'NONE', #5136, #8851, #3379 ) ;
#9878 = CARTESIAN_POINT ( 'NONE',  ( 25.00000000000000355, 570.2996408614167194, -31.99999999999998579 ) ) ;
#9879 = LINE ( 'NONE', #227, #10582 ) ;
#9880 = LINE ( 'NONE', #5909, #3496 ) ;
#9881 = CARTESIAN_POINT ( 'NONE',  ( 9.450654096908945471E-15, 44.95265997413478942, 75.00000000000001421 ) ) ;
#9882 = CARTESIAN_POINT ( 'NONE',  ( 140.0000000000011369, 225.0000000000000853, 25.00000000000000000 ) ) ;
#9883 = CARTESIAN_POINT ( 'NONE',  ( -2.708734125000000770, 113.8749999986343937, -1.121994411437818639 ) ) ;
#9884 = VERTEX_POINT ( 'NONE', #917 ) ;
#9885 = DIRECTION ( 'NONE',  ( 0.000000000000000000, 0.000000000000000000, 1.000000000000000000 ) ) ;
#9886 = TOROIDAL_SURFACE ( 'NONE', #3528, 110.0000000000000284, 5.000000000000000000 ) ;
#9887 = EDGE_CURVE ( 'NONE', #12341, #3922, #7577, .T. ) ;
#9888 = EDGE_CURVE ( 'NONE', #828, #10546, #8382, .T. ) ;
#9889 = B_SPLINE_CURVE_WITH_KNOTS ( 'NONE', 3,
 ( #11870, #4249, #1513, #1386 ),
 .UNSPECIFIED., .F., .F.,
 ( 4, 4 ),
 ( 0.000000000000000000, 0.002955678282115209009 ),
 .UNSPECIFIED. ) ;
#9890 = ORIENTED_EDGE ( 'NONE', *, *, #11848, .T. ) ;
#9891 = CARTESIAN_POINT ( 'NONE',  ( 7.594472908538985045, 34.78349364905407270, 79.50000000000000000 ) ) ;
#9892 = VERTEX_POINT ( 'NONE', #7518 ) ;
#9893 = CYLINDRICAL_SURFACE ( 'NONE', #11453, 15.00000000000000000 ) ;
#9894 = CARTESIAN_POINT ( 'NONE',  ( 74.62285592809365653, 17.63426063501363927, -24.41804092124679570 ) ) ;
#9895 = ORIENTED_EDGE ( 'NONE', *, *, #2955, .T. ) ;
#9896 = DIRECTION ( 'NONE',  ( 0.000000000000000000, 1.000000000000000000, 0.000000000000000000 ) ) ;
#9897 = ADVANCED_FACE ( 'NONE', ( #4586, #9375 ), #5534, .F. ) ;
#9898 = CARTESIAN_POINT ( 'NONE',  ( -30.56632211525506904, 87.12700276260751764, -8.880229275382255594 ) ) ;
#9899 = CONTEXT_DEPENDENT_SHAPE_REPRESENTATION ( #5739, #4098 ) ;
#9900 = ORIENTED_EDGE ( 'NONE', *, *, #1958, .F. ) ;
#9901 = CARTESIAN_POINT ( 'NONE',  ( -3.250000000000000444, 113.4375000000000000, 1.346194077712559167 ) ) ;
#9902 = EDGE_CURVE ( 'NONE', #7192, #7928, #9432, .T. ) ;
#9903 = EDGE_CURVE ( 'NONE', #9573, #11089, #8563, .T. ) ;
#9904 = ORIENTED_EDGE ( 'NONE', *, *, #997, .F. ) ;
#9905 = CARTESIAN_POINT ( 'NONE',  ( 31.69148534550512863, 87.00819463772768358, 8.674447566738409776 ) ) ;
#9906 = LINE ( 'NONE', #561, #6236 ) ;
#9907 = ORIENTED_EDGE ( 'NONE', *, *, #8589, .T. ) ;
#9908 = CARTESIAN_POINT ( 'NONE',  ( -1.190781129305471087, 30.00000000000008882, 75.00000000000001421 ) ) ;
#9909 = CARTESIAN_POINT ( 'NONE',  ( -9.726035167149728267, 35.21650635094616888, 79.50000000000000000 ) ) ;
#9910 = VERTEX_POINT ( 'NONE', #3654 ) ;
#9911 =( GEOMETRIC_REPRESENTATION_CONTEXT ( 3 ) GLOBAL_UNCERTAINTY_ASSIGNED_CONTEXT ( ( #3777 ) ) GLOBAL_UNIT_ASSIGNED_CONTEXT ( ( #3645, #6572, #3701 ) ) REPRESENTATION_CONTEXT ( 'NONE', 'WORKASPACE' ) );
#9912 = LINE ( 'NONE', #11805, #7274 ) ;
#9913 = CARTESIAN_POINT ( 'NONE',  ( 75.20175883194669098, 43.43544396156184462, -23.64678730934253537 ) ) ;
#9914 = CARTESIAN_POINT ( 'NONE',  ( 2.500000000000000000, 0.000000000000000000, 2.041999999999999815 ) ) ;
#9915 = ADVANCED_FACE ( 'NONE', ( #7638 ), #12323, .T. ) ;
#9916 = EDGE_LOOP ( 'NONE', ( #10806, #5674, #1009, #10908 ) ) ;
#9917 = CARTESIAN_POINT ( 'NONE',  ( -8.500000000000000000, 122.5000000000000000, 6.164414002968973350 ) ) ;
#9918 = CARTESIAN_POINT ( 'NONE',  ( 70.81305327821827689, 19.15123444475166181, 24.93520811514207836 ) ) ;
#9919 = AXIS2_PLACEMENT_3D ( 'NONE', #981, #2907, #10507 ) ;
#9920 = ORIENTED_EDGE ( 'NONE', *, *, #2843, .T. ) ;
#9921 = DIRECTION ( 'NONE',  ( 0.000000000000000000, 0.000000000000000000, 1.000000000000000000 ) ) ;
#9922 = DIRECTION ( 'NONE',  ( -0.5000000000000006661, -0.8660254037844383745, 0.000000000000000000 ) ) ;
#9923 = EDGE_LOOP ( 'NONE', ( #4043, #7954, #2240, #8770 ) ) ;
#9924 = DIRECTION ( 'NONE',  ( 0.000000000000000000, 0.000000000000000000, -1.000000000000000000 ) ) ;
#9925 = CARTESIAN_POINT ( 'NONE',  ( 70.44624282194196496, 46.67604154196500588, 25.73656789697686165 ) ) ;
#9926 = ORIENTED_EDGE ( 'NONE', *, *, #5822, .F. ) ;
#9927 = CYLINDRICAL_SURFACE ( 'NONE', #850, 9.999999999999998224 ) ;
#9928 = CARTESIAN_POINT ( 'NONE',  ( -3.250000000000000444, 112.3749999972688158, 3.980102097228898231E-16 ) ) ;
#9929 = EDGE_CURVE ( 'NONE', #6802, #2738, #6709, .T. ) ;
#9930 = CARTESIAN_POINT ( 'NONE',  ( 9.942549119892413856, 23.28349364905404428, 79.50000000000000000 ) ) ;
#9931 = FACE_OUTER_BOUND ( 'NONE', #5240, .T. ) ;
#9932 = ORIENTED_EDGE ( 'NONE', *, *, #3703, .T. ) ;
#9933 = EDGE_LOOP ( 'NONE', ( #2735, #5733 ) ) ;
#9934 = AXIS2_PLACEMENT_3D ( 'NONE', #7962, #553, #1311 ) ;
#9935 = DIRECTION ( 'NONE',  ( -0.000000000000000000, -1.000000000000000000, -0.000000000000000000 ) ) ;
#9936 = DIRECTION ( 'NONE',  ( 0.000000000000000000, 0.8660254037844407060, 0.4999999999999965583 ) ) ;
#9937 = FACE_OUTER_BOUND ( 'NONE', #4074, .T. ) ;
#9938 = CARTESIAN_POINT ( 'NONE',  ( -12.57411137850301763, 23.71650635094618664, 79.50000000000000000 ) ) ;
#9939 = DIRECTION ( 'NONE',  ( 1.000000000000000000, -0.000000000000000000, 0.000000000000000000 ) ) ;
#9940 = CARTESIAN_POINT ( 'NONE',  ( 2.708734124999999882, 114.5624999986344079, 0.000000000000000000 ) ) ;
#9941 = CARTESIAN_POINT ( 'NONE',  ( 165.0000000000011369, 225.0000000000000853, 20.00000000000000000 ) ) ;
#9942 = CARTESIAN_POINT ( 'NONE',  ( 71.39985347493269785, 11.04390332592970481, -22.96547907468803373 ) ) ;
#9943 = CARTESIAN_POINT ( 'NONE',  ( -2.708734125000000326, 111.8124999986344079, 3.317242575922457132E-16 ) ) ;
#9944 = ADVANCED_FACE ( 'NONE', ( #2904 ), #9495, .F. ) ;
#9945 = AXIS2_PLACEMENT_3D ( 'NONE', #7295, #2429, #432 ) ;
#9946 = APPLICATION_CONTEXT ( 'automotive_design' ) ;
#9947 = ORIENTED_EDGE ( 'NONE', *, *, #10347, .F. ) ;
#9948 = DIRECTION ( 'NONE',  ( -0.7236679289129653858, 0.000000000000000000, -0.6901483381584129218 ) ) ;
#9949 = ADVANCED_FACE ( 'NONE', ( #10377 ), #7461, .T. ) ;
#9950 = ORIENTED_EDGE ( 'NONE', *, *, #9197, .F. ) ;
#9951 = AXIS2_PLACEMENT_3D ( 'NONE', #6037, #11015, #10950 ) ;
#9952 = DIRECTION ( 'NONE',  ( 0.000000000000000000, 1.000000000000000000, 0.000000000000000000 ) ) ;
#9953 = EDGE_LOOP ( 'NONE', ( #2793, #10449, #5186 ) ) ;
#9954 = AXIS2_PLACEMENT_3D ( 'NONE', #523, #7132, #8795 ) ;
#9955 = DIRECTION ( 'NONE',  ( -1.000000000000000000, 0.000000000000000000, 0.000000000000000000 ) ) ;
#9956 = CARTESIAN_POINT ( 'NONE',  ( 3.250000000000000444, 113.9374999972688016, 1.346194077712559167 ) ) ;
#9957 = ORIENTED_EDGE ( 'NONE', *, *, #3582, .T. ) ;
#9958 = CYLINDRICAL_SURFACE ( 'NONE', #79, 5.000000000000000888 ) ;
#9959 = CARTESIAN_POINT ( 'NONE',  ( 0.000000000000000000, 40.00000000000009237, -20.00000000000000000 ) ) ;
#9960 = EDGE_CURVE ( 'NONE', #9490, #3926, #9780, .T. ) ;
#9961 = ORIENTED_EDGE ( 'NONE', *, *, #323, .T. ) ;
#9962 = CARTESIAN_POINT ( 'NONE',  ( -3.250000000000001776, 113.5625000000000000, -1.346194077712558279 ) ) ;
#9963 = AXIS2_PLACEMENT_3D ( 'NONE', #7624, #10300, #1888 ) ;
#9964 = EDGE_CURVE ( 'NONE', #5388, #1747, #202, .T. ) ;
#9965 = ORIENTED_EDGE ( 'NONE', *, *, #1779, .T. ) ;
#9966 = CIRCLE ( 'NONE', #10569, 10.00000000000000178 ) ;
#9967 = DIRECTION ( 'NONE',  ( 2.213536252433181072E-16, 0.000000000000000000, 1.000000000000000000 ) ) ;
#9968 = DIRECTION ( 'NONE',  ( 1.000000000000000000, 0.000000000000000000, -0.000000000000000000 ) ) ;
#9969 = VERTEX_POINT ( 'NONE', #12265 ) ;
#9970 = CARTESIAN_POINT ( 'NONE',  ( 2.081899558550500280E-15, 122.0000000000000000, -17.00000000000000000 ) ) ;
#9971 = DIRECTION ( 'NONE',  ( 0.000000000000000000, 1.000000000000000000, 0.000000000000000000 ) ) ;
#9972 = CIRCLE ( 'NONE', #185, 4.250000000000000000 ) ;
#9973 = VERTEX_POINT ( 'NONE', #26 ) ;
#9974 = ADVANCED_FACE ( 'NONE', ( #2653, #5780 ), #4837, .T. ) ;
#9975 = EDGE_CURVE ( 'NONE', #1004, #6843, #7177, .T. ) ;
#9976 = CARTESIAN_POINT ( 'NONE',  ( 165.0000000000011369, 230.0000000000000853, 20.00000000000000000 ) ) ;
#9977 = CARTESIAN_POINT ( 'NONE',  ( 74.62554477486000337, 42.37232431907235508, -24.41456952963950400 ) ) ;
#9978 = FACE_OUTER_BOUND ( 'NONE', #9221, .T. ) ;
#9979 = ORIENTED_EDGE ( 'NONE', *, *, #5403, .F. ) ;
#9980 = DIRECTION ( 'NONE',  ( 1.000000000000000000, 0.000000000000000000, 0.000000000000000000 ) ) ;
#9981 = CIRCLE ( 'NONE', #9377, 15.00000000000000000 ) ;
#9982 = CARTESIAN_POINT ( 'NONE',  ( 70.10024745330821361, 14.62972355300540173, 26.66438925502398405 ) ) ;
#9983 = AXIS2_PLACEMENT_3D ( 'NONE', #9379, #672, #4653 ) ;
#9984 = ORIENTED_EDGE ( 'NONE', *, *, #4907, .T. ) ;
#9985 = CARTESIAN_POINT ( 'NONE',  ( 74.75803814165917061, 17.33402007532147593, 24.24257051231691307 ) ) ;
#9986 = LINE ( 'NONE', #2325, #1291 ) ;
#9987 = ORIENTED_EDGE ( 'NONE', *, *, #1907, .F. ) ;
#9988 = CARTESIAN_POINT ( 'NONE',  ( 2.298097038856279806, 111.1250000000000000, 2.298097038856279806 ) ) ;
#9989 = CARTESIAN_POINT ( 'NONE',  ( 71.40290628601371736, 44.01905189704749688, 23.11746242201492052 ) ) ;
#9990 = VERTEX_POINT ( 'NONE', #10564 ) ;
#9991 = DIRECTION ( 'NONE',  ( 0.000000000000000000, 0.000000000000000000, 1.000000000000000000 ) ) ;
#9992 = CARTESIAN_POINT ( 'NONE',  ( 3.061616997868383043E-15, 65.00000000000000000, -25.00000000000000000 ) ) ;
#9993 = DIRECTION ( 'NONE',  ( 1.224646799147352714E-16, 0.000000000000000000, -1.000000000000000000 ) ) ;
#9994 = CARTESIAN_POINT ( 'NONE',  ( 2.298097038856278918, 114.7499999972688158, -2.298097038856279806 ) ) ;
#9995 = ORIENTED_EDGE ( 'NONE', *, *, #11977, .T. ) ;
#9996 = ORIENTED_EDGE ( 'NONE', *, *, #5332, .T. ) ;
#9997 = EDGE_CURVE ( 'NONE', #6378, #5388, #5028, .T. ) ;
#9998 = EDGE_CURVE ( 'NONE', #3427, #6619, #8758, .T. ) ;
#9999 = AXIS2_PLACEMENT_3D ( 'NONE', #11511, #4899, #5714 ) ;
#10000 = UNCERTAINTY_MEASURE_WITH_UNIT (LENGTH_MEASURE( 1.000000000000000082E-05 ), #7020, 'distance_accuracy_value', 'NONE');
#10001 = FACE_BOUND ( 'NONE', #5396, .T. ) ;
#10002 = DIRECTION ( 'NONE',  ( -0.000000000000000000, -1.000000000000000000, -0.000000000000000000 ) ) ;
#10004 = EDGE_CURVE ( 'NONE', #8739, #5619, #1800, .T. ) ;
#10003 = LINE ( 'NONE', #9878, #8423 ) ;
#10005 = CARTESIAN_POINT ( 'NONE',  ( 0.000000000000000000, 275.0000000000000000, 0.000000000000000000 ) ) ;
#10006 = LINE ( 'NONE', #11077, #5891 ) ;
#10007 = DIRECTION ( 'NONE',  ( 0.000000000000000000, 0.000000000000000000, -1.000000000000000000 ) ) ;
#10008 = CARTESIAN_POINT ( 'NONE',  ( 11.76612666199932811, 22.42800671064738793, 74.07172750083992696 ) ) ;
#10009 = LINE ( 'NONE', #8076, #3273 ) ;
#10010 = CARTESIAN_POINT ( 'NONE',  ( 2.708734125000000326, 111.3749999986344221, 1.121994411437818862 ) ) ;
#10011 = AXIS2_PLACEMENT_3D ( 'NONE', #4670, #4610, #7541 ) ;
#10012 = CARTESIAN_POINT ( 'NONE',  ( 90.45849111412074706, 275.0000000000000000, 86.26854226980164242 ) ) ;
#10013 = CARTESIAN_POINT ( 'NONE',  ( 89.80805993797383735, 275.0000000000000000, 81.82974571984303225 ) ) ;
#10014 = VERTEX_POINT ( 'NONE', #150 ) ;
#10015 = VECTOR ( 'NONE', #11397, 1000.000000000000000 ) ;
#10016 = CARTESIAN_POINT ( 'NONE',  ( -0.9407811293054709756, 42.99759593155604875, 80.00000000000000000 ) ) ;
#10017 = ORIENTED_EDGE ( 'NONE', *, *, #749, .F. ) ;
#10018 = CARTESIAN_POINT ( 'NONE',  ( 0.000000000000000000, 216.0365690573663926, 0.000000000000000000 ) ) ;
#10019 = CARTESIAN_POINT ( 'NONE',  ( -119.9399947101603772, 275.0000000000000000, 35.20508015793608081 ) ) ;
#10020 = ORIENTED_EDGE ( 'NONE', *, *, #7299, .T. ) ;
#10021 = DIRECTION ( 'NONE',  ( 0.000000000000000000, 0.000000000000000000, 1.000000000000000000 ) ) ;
#10022 = ADVANCED_BREP_SHAPE_REPRESENTATION ( '', ( #482, #1612 ), #10763 ) ;
#10023 = DIRECTION ( 'NONE',  ( 0.000000000000000000, 0.000000000000000000, 1.000000000000000000 ) ) ;
#10024 = ORIENTED_EDGE ( 'NONE', *, *, #9022, .F. ) ;
#10025 = CARTESIAN_POINT ( 'NONE',  ( 72.02465572632021917, 49.73463885619487002, -20.91766802171319029 ) ) ;
#10026 = VECTOR ( 'NONE', #7331, 1000.000000000000114 ) ;
#10027 = ORIENTED_EDGE ( 'NONE', *, *, #4115, .F. ) ;
#10028 = EDGE_CURVE ( 'NONE', #6205, #686, #3149, .T. ) ;
#10029 = LINE ( 'NONE', #4063, #355 ) ;
#10030 = CARTESIAN_POINT ( 'NONE',  ( -2.298097038856279806, 114.4999999972688158, -2.298097038856279362 ) ) ;
#10031 = ORIENTED_EDGE ( 'NONE', *, *, #7015, .T. ) ;
#10032 = VERTEX_POINT ( 'NONE', #213 ) ;
#10033 = DIRECTION ( 'NONE',  ( 0.000000000000000000, 1.000000000000000000, 0.000000000000000000 ) ) ;
#10034 = DIRECTION ( 'NONE',  ( 0.9717889794219071176, 0.000000000000000000, -0.2358520287683112393 ) ) ;
#10035 = VERTEX_POINT ( 'NONE', #11639 ) ;
#10036 = FACE_OUTER_BOUND ( 'NONE', #11673, .T. ) ;
#10037 = VECTOR ( 'NONE', #5299, 1000.000000000000000 ) ;
#10038 = CARTESIAN_POINT ( 'NONE',  ( 1.163414459189985959E-14, 290.0000000000000568, -95.00000000000002842 ) ) ;
#10039 = EDGE_LOOP ( 'NONE', ( #8121, #7960, #8431, #12211, #10500 ) ) ;
#10040 = CARTESIAN_POINT ( 'NONE',  ( -1.915364268218908927, 110.9374999986344079, 1.915364268218909150 ) ) ;
#10041 = CARTESIAN_POINT ( 'NONE',  ( 69.65391855624119444, 17.33976117116340632, 27.80917345409739383 ) ) ;
#10042 = ADVANCED_FACE ( 'NONE', ( #7934 ), #2200, .T. ) ;
#10043 = TOROIDAL_SURFACE ( 'NONE', #3478, 80.00000000000001421, 5.000000000000000000 ) ;
#10044 = EDGE_LOOP ( 'NONE', ( #9768, #352, #1916, #7845, #4319 ) ) ;
#10045 = CARTESIAN_POINT ( 'NONE',  ( 74.40577577445179713, 18.24918190538344120, 24.69584740025122471 ) ) ;
#10046 = DIRECTION ( 'NONE',  ( -0.000000000000000000, 1.000000000000000000, -0.000000000000000000 ) ) ;
#10047 = ORIENTED_EDGE ( 'NONE', *, *, #2787, .F. ) ;
#10048 = CARTESIAN_POINT ( 'NONE',  ( 3.122849337825750222E-15, 87.00000000000000000, 25.50000000000000000 ) ) ;
#10049 = CARTESIAN_POINT ( 'NONE',  ( 71.89872685388525042, 44.94434660361613254, 21.44363277848733063 ) ) ;
#10050 = ORIENTED_EDGE ( 'NONE', *, *, #2156, .T. ) ;
#10051 = CARTESIAN_POINT ( 'NONE',  ( 5.091510485526399954, 41.38124826485281460, 80.00000000000000000 ) ) ;
#10052 = FACE_OUTER_BOUND ( 'NONE', #10774, .T. ) ;
#10053 = CARTESIAN_POINT ( 'NONE',  ( 1.658621287961228566E-16, 112.5624999986344079, 2.708734125000000326 ) ) ;
#10054 = AXIS2_PLACEMENT_3D ( 'NONE', #7335, #793, #11952 ) ;
#10055 =( BOUNDED_SURFACE ( )  B_SPLINE_SURFACE ( 3, 2, ( 
 ( #7750, #201, #9610 ),
 ( #7690, #1150, #1028 ),
 ( #75, #3892, #1087 ),
 ( #4890, #8678, #4370 ),
 ( #5080, #11811, #7122 ),
 ( #11871, #326, #3199 ),
 ( #2510, #6999, #573 ),
 ( #2378, #1331, #3322 ),
 ( #8856, #10920, #7061 ),
 ( #10985, #9796, #11931 ),
 ( #4250, #10858, #511 ),
 ( #3385, #8170, #5198 ),
 ( #6188, #383, #3255 ),
 ( #11993, #1269, #1514 ),
 ( #9036, #7983, #4132 ),
 ( #9982, #4311, #1452 ),
 ( #8916, #11049, #3449 ),
 ( #5141, #7249, #7923 ),
 ( #2321, #5257, #6128 ),
 ( #11741, #2449, #6252 ),
 ( #10041, #5319, #8105 ),
 ( #1387, #7185, #8977 ),
 ( #10798, #9918, #447 ),
 ( #8045, #6066, #9096 ),
 ( #2258, #9855, #4192 ),
 ( #9344, #12179, #3509 ) ),
 .UNSPECIFIED., .F., .F., .F. ) 
 B_SPLINE_SURFACE_WITH_KNOTS ( ( 4, 2, 2, 2, 2, 2, 2, 2, 2, 2, 2, 2, 4 ),
 ( 3, 3 ),
 ( 0.006933106248791173071, 0.008937828180681107321, 0.009940189146626074446, 0.01094255011257104157, 0.01294727204446097582, 0.01394963301040594295, 0.01495199397635090834, 0.01695671590824084085, 0.01795907687418580798, 0.01896143784013077510, 0.02096615977202070935, 0.02196852073796567648, 0.02297088170391064360 ),
 ( 0.000000000000000000, 1.000000000000000000 ),
 .UNSPECIFIED. ) 
 GEOMETRIC_REPRESENTATION_ITEM ( )  RATIONAL_B_SPLINE_SURFACE ( (
 ( 1.000000000000000000, 0.7071067811865475727, 1.000000000000000000),
 ( 1.000000000000000000, 0.7129067084832076961, 1.000000000000000000),
 ( 1.000000000000000000, 0.7190912265161553130, 1.000000000000000000),
 ( 1.000000000000000000, 0.7288225095607152593, 1.000000000000000000),
 ( 1.000000000000000000, 0.7321420440090222748, 1.000000000000000000),
 ( 1.000000000000000000, 0.7389120750275648408, 1.000000000000000000),
 ( 1.000000000000000000, 0.7423805904412675849, 1.000000000000000000),
 ( 1.000000000000000000, 0.7527643000948556207, 1.000000000000000000),
 ( 1.000000000000000000, 0.7596816647250912435, 1.000000000000000000),
 ( 1.000000000000000000, 0.7698812226851532436, 1.000000000000000000),
 ( 1.000000000000000000, 0.7732515396852113199, 1.000000000000000000),
 ( 1.000000000000000000, 0.7799012531313251895, 1.000000000000000000),
 ( 1.000000000000000000, 0.7831631659391242728, 1.000000000000000000),
 ( 1.000000000000000000, 0.7925626959609731736, 1.000000000000000000),
 ( 1.000000000000000000, 0.7983806636883555852, 1.000000000000000000),
 ( 1.000000000000000000, 0.8062586255457115936, 1.000000000000000000),
 ( 1.000000000000000000, 0.8087533637821711086, 1.000000000000000000),
 ( 1.000000000000000000, 0.8133656295006761461, 1.000000000000000000),
 ( 1.000000000000000000, 0.8154682471119866216, 1.000000000000000000),
 ( 1.000000000000000000, 0.8211473929488716239, 1.000000000000000000),
 ( 1.000000000000000000, 0.8241004955462830628, 1.000000000000000000),
 ( 1.000000000000000000, 0.8271253898583807995, 1.000000000000000000),
 ( 1.000000000000000000, 0.8278923858075547537, 1.000000000000000000),
 ( 1.000000000000000000, 0.8289041354387917115, 1.000000000000000000),
 ( 1.000000000000000000, 0.8291560334507810381, 1.000000000000000000),
 ( 1.000000000000000000, 0.8291561975888499525, 1.000000000000000000) ) ) 
 REPRESENTATION_ITEM ( '' )  SURFACE ( )  );
#10056 = ADVANCED_FACE ( 'NONE', ( #5959 ), #3088, .F. ) ;
#10057 = ORIENTED_EDGE ( 'NONE', *, *, #537, .F. ) ;
#10058 = AXIS2_PLACEMENT_3D ( 'NONE', #9369, #4701, #10436 ) ;
#10059 = CARTESIAN_POINT ( 'NONE',  ( 0.000000000000000000, 170.0000000000000000, 2.649999999999993694 ) ) ;
#10060 = DIRECTION ( 'NONE',  ( 0.000000000000000000, 0.000000000000000000, 1.000000000000000000 ) ) ;
#10061 = DIRECTION ( 'NONE',  ( 1.000000000000000000, -1.040834085586083310E-14, 0.000000000000000000 ) ) ;
#10062 = CARTESIAN_POINT ( 'NONE',  ( -1.440781129305282571, 17.00000000000009592, 80.00000000000000000 ) ) ;
#10063 = CIRCLE ( 'NONE', #7087, 2.649999999999987477 ) ;
#10064 = CARTESIAN_POINT ( 'NONE',  ( -27.95322648060789206, 86.18856968700909249, -11.45194355884139448 ) ) ;
#10065 = LINE ( 'NONE', #2225, #3117 ) ;
#10066 = CARTESIAN_POINT ( 'NONE',  ( 13.80921887069453469, 29.53523948059399018, 73.71774192269633375 ) ) ;
#10067 = CARTESIAN_POINT ( 'NONE',  ( 70.63701798748765270, 12.74415835139032716, -25.20839359252510548 ) ) ;
#10068 = EDGE_CURVE ( 'NONE', #9474, #9777, #824, .T. ) ;
#10069 = CARTESIAN_POINT ( 'NONE',  ( -1.346194077712560944, 111.6875000000000000, -3.249999999999999556 ) ) ;
#10070 = CARTESIAN_POINT ( 'NONE',  ( -14.19078112930532853, 30.25000000000008882, 80.00000000000000000 ) ) ;
#10071 = PLANE ( 'NONE',  #3403 ) ;
#10072 = VECTOR ( 'NONE', #2092, 1000.000000000000000 ) ;
#10073 = CYLINDRICAL_SURFACE ( 'NONE', #11596, 75.00000000000001421 ) ;
#10074 = ORIENTED_EDGE ( 'NONE', *, *, #10536, .F. ) ;
#10075 = CARTESIAN_POINT ( 'NONE',  ( 77.12313347048127810, 44.96937891963703748, 20.63522338802521716 ) ) ;
#10076 = ORIENTED_EDGE ( 'NONE', *, *, #2181, .F. ) ;
#10077 = CYLINDRICAL_SURFACE ( 'NONE', #1693, 5.000000000000000888 ) ;
#10078 = CARTESIAN_POINT ( 'NONE',  ( 77.29386075506074860, 15.00000000000009059, -20.32108226578737842 ) ) ;
#10079 = VERTEX_POINT ( 'NONE', #8749 ) ;
#10080 = DIRECTION ( 'NONE',  ( 1.224646799147353454E-16, 0.000000000000000000, -1.000000000000000000 ) ) ;
#10081 = LINE ( 'NONE', #7039, #9332 ) ;
#10082 = ORIENTED_EDGE ( 'NONE', *, *, #8578, .T. ) ;
#10083 = DIRECTION ( 'NONE',  ( -0.8660254037844457020, -0.4999999999999877875, 0.000000000000000000 ) ) ;
#10084 = ORIENTED_EDGE ( 'NONE', *, *, #3661, .F. ) ;
#10085 = FACE_OUTER_BOUND ( 'NONE', #1058, .T. ) ;
#10086 = CARTESIAN_POINT ( 'NONE',  ( -3.250000000000000444, 114.3124999972687874, 1.346194077712559167 ) ) ;
#10087 = ORIENTED_EDGE ( 'NONE', *, *, #3001, .F. ) ;
#10088 = CARTESIAN_POINT ( 'NONE',  ( 5.525725221640833240, 18.86666975080242992, 79.50000000000000000 ) ) ;
#10089 = CARTESIAN_POINT ( 'NONE',  ( -31.18707241436460365, 75.10640101998821194, 7.566984156997462740 ) ) ;
#10090 = ORIENTED_EDGE ( 'NONE', *, *, #7765, .F. ) ;
#10091 = DIRECTION ( 'NONE',  ( 0.000000000000000000, 1.000000000000000000, 0.000000000000000000 ) ) ;
#10092 = CARTESIAN_POINT ( 'NONE',  ( 77.45966692414833688, 10.00000000000009237, 20.00000000000000000 ) ) ;
#10093 = CARTESIAN_POINT ( 'NONE',  ( -12.44911137850311000, 23.50000000000024158, 80.00000000000000000 ) ) ;
#10094 = ORIENTED_EDGE ( 'NONE', *, *, #11885, .F. ) ;
#10095 = DIRECTION ( 'NONE',  ( 0.000000000000000000, 0.000000000000000000, 1.000000000000000000 ) ) ;
#10096 = EDGE_CURVE ( 'NONE', #7629, #872, #10627, .T. ) ;
#10097 = DIRECTION ( 'NONE',  ( 0.000000000000000000, 0.000000000000000000, 1.000000000000000000 ) ) ;
#10098 = ADVANCED_FACE ( 'NONE', ( #11575 ), #3029, .T. ) ;
#10099 = ORIENTED_EDGE ( 'NONE', *, *, #2719, .T. ) ;
#10100 = AXIS2_PLACEMENT_3D ( 'NONE', #8216, #11100, #3438 ) ;
#10101 = CARTESIAN_POINT ( 'NONE',  ( 0.000000000000000000, 75.00000000000000000, 0.000000000000000000 ) ) ;
#10102 =( GEOMETRIC_REPRESENTATION_CONTEXT ( 3 ) GLOBAL_UNCERTAINTY_ASSIGNED_CONTEXT ( ( #922 ) ) GLOBAL_UNIT_ASSIGNED_CONTEXT ( ( #12072, #5334, #12256 ) ) REPRESENTATION_CONTEXT ( 'NONE', 'WORKASPACE' ) );
#10103 = DIRECTION ( 'NONE',  ( 0.8660254037844399289, 0.4999999999999977796, 0.000000000000000000 ) ) ;
#10104 = ORIENTED_EDGE ( 'NONE', *, *, #6008, .T. ) ;
#10105 = LINE ( 'NONE', #2327, #1284 ) ;
#10106 = CARTESIAN_POINT ( 'NONE',  ( 69.77609205918946600, 43.60216921429233139, 27.50116345873387758 ) ) ;
#10107 = VERTEX_POINT ( 'NONE', #5091 ) ;
#10108 = FACE_OUTER_BOUND ( 'NONE', #9338, .T. ) ;
#10109 = CARTESIAN_POINT ( 'NONE',  ( -2.708734125000000326, 113.8124999986344079, 3.317242575922457132E-16 ) ) ;
#10110 = CARTESIAN_POINT ( 'NONE',  ( -1.915364268218908927, 110.9374999986344079, 1.915364268218909150 ) ) ;
#10111 = CIRCLE ( 'NONE', #4747, 25.00000000000000000 ) ;
#10112 = EDGE_CURVE ( 'NONE', #3229, #7980, #11699, .T. ) ;
#10113 = STYLED_ITEM ( 'NONE', ( #12232 ), #6020 ) ;
#10114 = ORIENTED_EDGE ( 'NONE', *, *, #3072, .T. ) ;
#10115 = ORIENTED_EDGE ( 'NONE', *, *, #4601, .F. ) ;
#10116 = SURFACE_SIDE_STYLE ('',( #4575 ) ) ;
#10117 = EDGE_CURVE ( 'NONE', #9034, #1793, #1414, .T. ) ;
#10118 = CARTESIAN_POINT ( 'NONE',  ( -16.19078112930547064, 30.00000000000008882, 80.00000000000000000 ) ) ;
#10119 = DIRECTION ( 'NONE',  ( -0.7071067811865440200, 0.7071067811865510144, 0.000000000000000000 ) ) ;
#10120 = CARTESIAN_POINT ( 'NONE',  ( 45.35898384862240107, 65.26794919243121740, -24.98076211353317078 ) ) ;
#10121 = CARTESIAN_POINT ( 'NONE',  ( -32.12519652190516695, 85.41823950547528455, -9.573483885151777173 ) ) ;
#10122 = CARTESIAN_POINT ( 'NONE',  ( -14.51674080820684054, 36.96222026613151002, 73.58288578104874489 ) ) ;
#10123 = CARTESIAN_POINT ( 'NONE',  ( 6.000000000000000888, 50.00000000000000000, 60.00000000000002132 ) ) ;
#10124 = EDGE_CURVE ( 'NONE', #12307, #2738, #3784, .T. ) ;
#10125 = EDGE_CURVE ( 'NONE', #421, #4699, #2913, .T. ) ;
#10126 = CARTESIAN_POINT ( 'NONE',  ( 9.184850993605150311E-15, 50.00000000000000000, 75.00000000000001421 ) ) ;
#10127 = CARTESIAN_POINT ( 'NONE',  ( 3.250000000000000444, 112.0624999999999858, 1.346194077712559389 ) ) ;
#10128 = CIRCLE ( 'NONE', #8534, 30.00000000000000355 ) ;
#10129 = LINE ( 'NONE', #10193, #4188 ) ;
#10130 = CIRCLE ( 'NONE', #8338, 4.250000000000000000 ) ;
#10131 = VECTOR ( 'NONE', #9967, 1000.000000000000000 ) ;
#10132 = COLOUR_RGB ( '', 0.09019608, 0.27058824, 0.51372549) ;
#10133 = CARTESIAN_POINT ( 'NONE',  ( 0.000000000000000000, 50.00000000000000000, 0.000000000000000000 ) ) ;
#10134 = ORIENTED_EDGE ( 'NONE', *, *, #7465, .T. ) ;
#10135 = DIRECTION ( 'NONE',  ( 0.000000000000000000, 1.000000000000000000, 0.000000000000000000 ) ) ;
#10136 = CARTESIAN_POINT ( 'NONE',  ( 75.00000000000001421, 40.00000000000009237, 20.00000000000000000 ) ) ;
#10137 = CARTESIAN_POINT ( 'NONE',  ( 76.05694877984106483, 15.60588465540594605, -22.40616324080664157 ) ) ;
#10138 = VERTEX_POINT ( 'NONE', #1650 ) ;
#10139 = DIRECTION ( 'NONE',  ( 0.000000000000000000, 0.000000000000000000, 1.000000000000000000 ) ) ;
#10140 = DIRECTION ( 'NONE',  ( 0.000000000000000000, 1.000000000000000000, 0.000000000000000000 ) ) ;
#10141 = ORIENTED_EDGE ( 'NONE', *, *, #9206, .T. ) ;
#10142 = CARTESIAN_POINT ( 'NONE',  ( 1.163414459189985959E-14, 265.0000000000000000, -95.00000000000002842 ) ) ;
#10143 = AXIS2_PLACEMENT_3D ( 'NONE', #73, #2017, #3951 ) ;
#10144 = AXIS2_PLACEMENT_3D ( 'NONE', #10644, #3923, #2924 ) ;
#10145 = ORIENTED_EDGE ( 'NONE', *, *, #3601, .T. ) ;
#10146 = EDGE_CURVE ( 'NONE', #4534, #11714, #9051, .T. ) ;
#10147 = EDGE_LOOP ( 'NONE', ( #6286, #819, #5554, #10968, #4140, #908 ) ) ;
#10148 = DIRECTION ( 'NONE',  ( 0.000000000000000000, 0.000000000000000000, 1.000000000000000000 ) ) ;
#10149 = DIRECTION ( 'NONE',  ( -0.000000000000000000, 1.000000000000000000, -0.000000000000000000 ) ) ;
#10150 = EDGE_LOOP ( 'NONE', ( #1450, #11087, #9496, #7772 ) ) ;
#10151 = DIRECTION ( 'NONE',  ( 0.5000000000000038858, 0.8660254037844363761, 0.000000000000000000 ) ) ;
#10152 = DIRECTION ( 'NONE',  ( 5.551115123125782702E-15, -0.4999999999999976685, -0.8660254037844399289 ) ) ;
#10153 = EDGE_LOOP ( 'NONE', ( #7323, #9428, #90 ) ) ;
#10154 = ADVANCED_FACE ( 'NONE', ( #9931 ), #3398, .F. ) ;
#10155 = DIRECTION ( 'NONE',  ( 1.000000000000000000, 0.000000000000000000, 0.000000000000000000 ) ) ;
#10156 = DIRECTION ( 'NONE',  ( 0.000000000000000000, 0.4999999999999990008, -0.8660254037844391517 ) ) ;
#10158 = DIRECTION ( 'NONE',  ( -0.2358520287683112115, 0.000000000000000000, -0.9717889794219070065 ) ) ;
#10157 = AXIS2_PLACEMENT_3D ( 'NONE', #7506, #6629, #1713 ) ;
#10159 = CARTESIAN_POINT ( 'NONE',  ( 1.346194077712557391, 111.0624999972687874, 3.250000000000002220 ) ) ;
#10160 = STYLED_ITEM ( 'NONE', ( #3215 ), #7202 ) ;
#10161 = ORIENTED_EDGE ( 'NONE', *, *, #3655, .F. ) ;
#10162 = LINE ( 'NONE', #5196, #5182 ) ;
#10163 = CARTESIAN_POINT ( 'NONE',  ( 0.000000000000000000, 75.00000000000000000, 0.000000000000000000 ) ) ;
#10164 = VECTOR ( 'NONE', #10657, 1000.000000000000000 ) ;
#10165 = ORIENTED_EDGE ( 'NONE', *, *, #11767, .T. ) ;
#10166 = ADVANCED_FACE ( 'NONE', ( #460 ), #4265, .T. ) ;
#10167 = LINE ( 'NONE', #9349, #1983 ) ;
#10168 = CARTESIAN_POINT ( 'NONE',  ( 0.000000000000000000, 87.00000000000000000, 0.000000000000000000 ) ) ;
#10169 = VERTEX_POINT ( 'NONE', #11315 ) ;
#10170 = DIRECTION ( 'NONE',  ( 1.000000000000000000, -0.000000000000000000, 0.000000000000000000 ) ) ;
#10171 = CARTESIAN_POINT ( 'NONE',  ( 71.95778018440438473, 49.67323215106386414, 21.14640536576772689 ) ) ;
#10172 = ORIENTED_EDGE ( 'NONE', *, *, #6635, .F. ) ;
#10173 = ADVANCED_FACE ( 'NONE', ( #11373 ), #3009, .T. ) ;
#10174 = CYLINDRICAL_SURFACE ( 'NONE', #7314, 17.00000000000000000 ) ;
#10175 = CARTESIAN_POINT ( 'NONE',  ( 1.121994411437819528, 112.1249999986343937, -2.708734124999999882 ) ) ;
#10176 = TOROIDAL_SURFACE ( 'NONE', #6998, 24.99999999999999645, 5.000000000000000000 ) ;
#10177 = CARTESIAN_POINT ( 'NONE',  ( 1.121994411437818862, 113.7499999986343937, 2.708734124999999882 ) ) ;
#10178 = CIRCLE ( 'NONE', #4812, 2.500000000000000888 ) ;
#10179 = VERTEX_POINT ( 'NONE', #11187 ) ;
#10180 = ADVANCED_FACE ( 'NONE', ( #6567, #2826 ), #12129, .T. ) ;
#10181 =( REPRESENTATION_RELATIONSHIP ('NONE','NONE', #3713, #12244 ) REPRESENTATION_RELATIONSHIP_WITH_TRANSFORMATION ( #10781 )SHAPE_REPRESENTATION_RELATIONSHIP( ) );
#10182 = CARTESIAN_POINT ( 'NONE',  ( 0.000000000000000000, 65.00000000000000000, 0.000000000000000000 ) ) ;
#10183 = DIRECTION ( 'NONE',  ( 0.000000000000000000, 0.000000000000000000, -1.000000000000000000 ) ) ;
#10184 = EDGE_CURVE ( 'NONE', #10179, #1960, #8307, .T. ) ;
#10185 = DIRECTION ( 'NONE',  ( 0.000000000000000000, 1.000000000000000000, 0.000000000000000000 ) ) ;
#10186 = DIRECTION ( 'NONE',  ( 0.000000000000000000, 1.000000000000000000, 0.000000000000000000 ) ) ;
#10187 = CARTESIAN_POINT ( 'NONE',  ( -28.52887280570637074, 85.15789473684209554, -9.723794007404263695 ) ) ;
#10188 = DIRECTION ( 'NONE',  ( 0.000000000000000000, 0.000000000000000000, 1.000000000000000000 ) ) ;
#10189 = DIRECTION ( 'NONE',  ( -1.000000000000000000, -0.000000000000000000, -0.000000000000000000 ) ) ;
#10190 = CARTESIAN_POINT ( 'NONE',  ( -25.00000000000000000, 345.0000000000000568, -59.99999999999999289 ) ) ;
#10191 = VERTEX_POINT ( 'NONE', #4691 ) ;
#10192 = CARTESIAN_POINT ( 'NONE',  ( -1.346194077712559389, 111.3125000000000142, 3.250000000000000444 ) ) ;
#10193 = CARTESIAN_POINT ( 'NONE',  ( 7.594472908538985045, 34.78349364905407270, 80.00000000000000000 ) ) ;
#10194 = AXIS2_PLACEMENT_3D ( 'NONE', #9617, #210, #11386 ) ;
#10195 = B_SPLINE_CURVE_WITH_KNOTS ( 'NONE', 3,
 ( #2223, #2401, #5966, #4277 ),
 .UNSPECIFIED., .F., .F.,
 ( 4, 4 ),
 ( 1.589900327696125378E-17, 0.001940928724149432009 ),
 .UNSPECIFIED. ) ;
#10196 = ADVANCED_FACE ( 'NONE', ( #1830 ), #10489, .T. ) ;
#10197 = CARTESIAN_POINT ( 'NONE',  ( 1.346194077712544956, 113.0624999972688016, 3.250000000000015543 ) ) ;
#10198 = VERTEX_POINT ( 'NONE', #5640 ) ;
#10199 = CARTESIAN_POINT ( 'NONE',  ( 2.112515728529184067E-15, 122.5000000000000000, -17.00000000000000000 ) ) ;
#10200 = CARTESIAN_POINT ( 'NONE',  ( -25.00000000000000000, 345.0000000000000568, -95.00000000000000000 ) ) ;
#10201 = DIRECTION ( 'NONE',  ( 0.000000000000000000, 1.000000000000000000, 0.000000000000000000 ) ) ;
#10202 = EDGE_LOOP ( 'NONE', ( #6505, #6790, #10387, #7247, #3901 ) ) ;
#10203 = AXIS2_PLACEMENT_3D ( 'NONE', #1440, #10846, #5129 ) ;
#10204 = CYLINDRICAL_SURFACE ( 'NONE', #3874, 100.0000000000000284 ) ;
#10205 = LINE ( 'NONE', #11340, #5962 ) ;
#10206 = EDGE_CURVE ( 'NONE', #9199, #5882, #7392, .T. ) ;
#10207 = ORIENTED_EDGE ( 'NONE', *, *, #9787, .T. ) ;
#10208 = DIRECTION ( 'NONE',  ( 1.000000000000000000, 0.000000000000000000, -1.065814103640150437E-14 ) ) ;
#10209 = AXIS2_PLACEMENT_3D ( 'NONE', #9691, #1167, #2161 ) ;
#10210 = ORIENTED_EDGE ( 'NONE', *, *, #7480, .F. ) ;
#10211 = DIRECTION ( 'NONE',  ( 1.000000000000000000, -0.000000000000000000, 1.224646799147353207E-16 ) ) ;
#10213 = ORIENTED_EDGE ( 'NONE', *, *, #7606, .T. ) ;
#10212 = CYLINDRICAL_SURFACE ( 'NONE', #5043, 3.250000000000000444 ) ;
#10214 = VERTEX_POINT ( 'NONE', #10424 ) ;
#10215 = CARTESIAN_POINT ( 'NONE',  ( 0.000000000000000000, 265.0000000000000000, 0.000000000000000000 ) ) ;
#10216 = FACE_OUTER_BOUND ( 'NONE', #8141, .T. ) ;
#10217 = ORIENTED_EDGE ( 'NONE', *, *, #12180, .F. ) ;
#10218 = DIRECTION ( 'NONE',  ( 0.000000000000000000, 0.000000000000000000, 1.000000000000000000 ) ) ;
#10219 = DIRECTION ( 'NONE',  ( -1.000000000000000000, -0.000000000000000000, -0.000000000000000000 ) ) ;
#10220 = DIRECTION ( 'NONE',  ( -1.000000000000000000, 0.000000000000000000, -0.000000000000000000 ) ) ;
#10221 = CIRCLE ( 'NONE', #4856, 70.00000000000001421 ) ;
#10222 = AXIS2_PLACEMENT_3D ( 'NONE', #10284, #5562, #10218 ) ;
#10223 = ORIENTED_EDGE ( 'NONE', *, *, #8299, .T. ) ;
#10224 = CARTESIAN_POINT ( 'NONE',  ( 1.121994411437819084, 112.3749999986344221, -2.708734124999999437 ) ) ;
#10225 = EDGE_CURVE ( 'NONE', #2329, #8617, #9297, .T. ) ;
#10226 = ADVANCED_FACE ( 'NONE', ( #841 ), #7388, .F. ) ;
#10227 = DIRECTION ( 'NONE',  ( 0.000000000000000000, 0.000000000000000000, 1.000000000000000000 ) ) ;
#10228 = EDGE_CURVE ( 'NONE', #4839, #11632, #9418, .T. ) ;
#10229 = VERTEX_POINT ( 'NONE', #5522 ) ;
#10230 = CARTESIAN_POINT ( 'NONE',  ( -1.440781129305282571, 17.00000000000009592, 80.00000000000000000 ) ) ;
#10231 = CARTESIAN_POINT ( 'NONE',  ( 0.000000000000000000, 50.00000000000008527, 0.000000000000000000 ) ) ;
#10232 = CIRCLE ( 'NONE', #7054, 30.00000000000000000 ) ;
#10233 = ORIENTED_EDGE ( 'NONE', *, *, #1779, .F. ) ;
#10234 = AXIS2_PLACEMENT_3D ( 'NONE', #7947, #3225, #7024 ) ;
#10235 = CARTESIAN_POINT ( 'NONE',  ( -1.346194077712542736, 112.6875000000000000, -3.250000000000017764 ) ) ;
#10236 = CARTESIAN_POINT ( 'NONE',  ( 0.000000000000000000, 106.9570738953063085, 0.000000000000000000 ) ) ;
#10237 = ORIENTED_EDGE ( 'NONE', *, *, #4726, .F. ) ;
#10238 = LINE ( 'NONE', #12065, #3716 ) ;
#10239 = DIRECTION ( 'NONE',  ( -0.5000000000000036637, -0.8660254037844364872, 0.000000000000000000 ) ) ;
#10240 = CARTESIAN_POINT ( 'NONE',  ( -5.970153145843347347E-16, 114.6249999972688158, -3.250000000000000444 ) ) ;
#10241 = ORIENTED_EDGE ( 'NONE', *, *, #5546, .T. ) ;
#10242 = CIRCLE ( 'NONE', #3278, 3.250000000000000444 ) ;
#10243 = ORIENTED_EDGE ( 'NONE', *, *, #4698, .T. ) ;
#10244 = AXIS2_PLACEMENT_3D ( 'NONE', #6442, #3632, #8479 ) ;
#10245 = CARTESIAN_POINT ( 'NONE',  ( -11.19078112930532498, 30.25000000000005684, 79.50000000000000000 ) ) ;
#10246 = CARTESIAN_POINT ( 'NONE',  ( 2.500000000000000000, 1.768423874527822459, -1.021000000000002794 ) ) ;
#10247 = CARTESIAN_POINT ( 'NONE',  ( 0.000000000000000000, 260.0000000000000000, 0.000000000000000000 ) ) ;
#10248 = AXIS2_PLACEMENT_3D ( 'NONE', #11681, #4070, #2014 ) ;
#10249 = DIRECTION ( 'NONE',  ( 0.000000000000000000, 1.000000000000000000, 0.000000000000000000 ) ) ;
#10250 = AXIS2_PLACEMENT_3D ( 'NONE', #5865, #9589, #9650 ) ;
#10251 = CARTESIAN_POINT ( 'NONE',  ( -27.57052686557075916, 86.63064495281066968, -11.84084938503495010 ) ) ;
#10252 = CARTESIAN_POINT ( 'NONE',  ( -10.60456947870001976, 41.68965759107759794, 74.24767693116807266 ) ) ;
#10253 = DIRECTION ( 'NONE',  ( 0.000000000000000000, -0.000000000000000000, 1.000000000000000000 ) ) ;
#10254 = EDGE_CURVE ( 'NONE', #6198, #12042, #3759, .T. ) ;
#10255 = EDGE_LOOP ( 'NONE', ( #2352, #5848, #37, #7255, #6834 ) ) ;
#10256 = CARTESIAN_POINT ( 'NONE',  ( -1.346194077712560944, 110.6875000000000000, -3.249999999999999556 ) ) ;
#10257 = DIRECTION ( 'NONE',  ( -1.000000000000000000, 3.469446951953611033E-15, 0.000000000000000000 ) ) ;
#10258 = EDGE_CURVE ( 'NONE', #3401, #5298, #6189, .T. ) ;
#10259 = AXIS2_PLACEMENT_3D ( 'NONE', #8743, #11509, #9677 ) ;
#10260 = CARTESIAN_POINT ( 'NONE',  ( 3.250000000000000444, 112.8749999972688158, 0.000000000000000000 ) ) ;
#10261 = TOROIDAL_SURFACE ( 'NONE', #9062, 2.700000000000000622, 0.2000000000000000111 ) ;
#10262 = ORIENTED_EDGE ( 'NONE', *, *, #11516, .T. ) ;
#10263 = LINE ( 'NONE', #5542, #11631 ) ;
#10264 = DIRECTION ( 'NONE',  ( -0.000000000000000000, -1.000000000000000000, -0.000000000000000000 ) ) ;
#10265 = DIRECTION ( 'NONE',  ( 1.000000000000000000, 0.000000000000000000, 0.000000000000000000 ) ) ;
#10266 = ORIENTED_EDGE ( 'NONE', *, *, #8323, .F. ) ;
#10267 = FACE_OUTER_BOUND ( 'NONE', #441, .T. ) ;
#10268 = AXIS2_PLACEMENT_3D ( 'NONE', #3276, #4090, #10632 ) ;
#10269 = CARTESIAN_POINT ( 'NONE',  ( 5.525725221640833240, 18.86666975080242992, 80.00000000000000000 ) ) ;
#10270 = EDGE_LOOP ( 'NONE', ( #3555, #11594, #5255, #12249 ) ) ;
#10271 = ADVANCED_FACE ( 'NONE', ( #2640 ), #6693, .T. ) ;
#10272 = DIRECTION ( 'NONE',  ( 0.000000000000000000, 1.000000000000000000, 0.000000000000000000 ) ) ;
#10273 = CIRCLE ( 'NONE', #327, 10.00000000000000178 ) ;
#10274 = EDGE_CURVE ( 'NONE', #3881, #3399, #11, .T. ) ;
#10275 = ORIENTED_EDGE ( 'NONE', *, *, #5181, .F. ) ;
#10276 = DIRECTION ( 'NONE',  ( 0.000000000000000000, 0.000000000000000000, -1.000000000000000000 ) ) ;
#10277 = LINE ( 'NONE', #9274, #4435 ) ;
#10278 = EDGE_LOOP ( 'NONE', ( #11227, #7302, #10241, #1742 ) ) ;
#10279 = VECTOR ( 'NONE', #5823, 1000.000000000000000 ) ;
#10280 = DIRECTION ( 'NONE',  ( 0.4999999999999981681, -0.8660254037844397068, 0.000000000000000000 ) ) ;
#10281 = CARTESIAN_POINT ( 'NONE',  ( -28.72281323269012887, 87.00000000000000000, -8.660254037844435260 ) ) ;
#10282 = ORIENTED_EDGE ( 'NONE', *, *, #433, .T. ) ;
#10283 = DIRECTION ( 'NONE',  ( 0.000000000000000000, 0.000000000000000000, 1.000000000000000000 ) ) ;
#10284 = CARTESIAN_POINT ( 'NONE',  ( 0.000000000000000000, 115.0000000000000142, 0.000000000000000000 ) ) ;
#10285 = DIRECTION ( 'NONE',  ( -1.000000000000000000, -0.000000000000000000, -0.000000000000000000 ) ) ;
#10286 = LINE ( 'NONE', #1815, #10977 ) ;
#10287 = EDGE_CURVE ( 'NONE', #9749, #9910, #4570, .T. ) ;
#10288 = ADVANCED_FACE ( 'NONE', ( #3638 ), #7447, .T. ) ;
#10289 = EDGE_LOOP ( 'NONE', ( #11400, #6637, #7728, #2968, #6358, #757, #2208, #2948 ) ) ;
#10290 = CARTESIAN_POINT ( 'NONE',  ( 1.915364268218909150, 112.6874999986344079, 1.915364268218909150 ) ) ;
#10291 = FACE_OUTER_BOUND ( 'NONE', #4029, .T. ) ;
#10292 = ORIENTED_EDGE ( 'NONE', *, *, #609, .F. ) ;
#10293 = CARTESIAN_POINT ( 'NONE',  ( 28.72281323269012532, 77.00000000000000000, -8.660254037844445918 ) ) ;
#10294 = CARTESIAN_POINT ( 'NONE',  ( -16.05603493625720546, 27.92803657533481498, 73.26122286506979719 ) ) ;
#10295 = EDGE_LOOP ( 'NONE', ( #5627, #10223, #2051, #4481 ) ) ;
#10296 = DIRECTION ( 'NONE',  ( 0.000000000000000000, 0.000000000000000000, 1.000000000000000000 ) ) ;
#10297 = CARTESIAN_POINT ( 'NONE',  ( -30.00000000000004263, 65.00000000000000000, 63.24555320336758513 ) ) ;
#10298 = ORIENTED_EDGE ( 'NONE', *, *, #11128, .T. ) ;
#10299 = CARTESIAN_POINT ( 'NONE',  ( 0.000000000000000000, -10.00000000000000000, 0.000000000000000000 ) ) ;
#10300 = DIRECTION ( 'NONE',  ( 0.000000000000000000, 0.000000000000000000, -1.000000000000000000 ) ) ;
#10301 = CARTESIAN_POINT ( 'NONE',  ( 1.658621287961228320E-16, 110.8124999986344079, 2.708734124999999882 ) ) ;
#10302 = LINE ( 'NONE', #10070, #7282 ) ;
#10303 = ORIENTED_EDGE ( 'NONE', *, *, #3630, .T. ) ;
#10304 = VERTEX_POINT ( 'NONE', #6514 ) ;
#10305 = AXIS2_PLACEMENT_3D ( 'NONE', #2186, #10332, #10276 ) ;
#10306 = CARTESIAN_POINT ( 'NONE',  ( -3.248205972160483255E-15, 151.7381927000421342, 0.000000000000000000 ) ) ;
#10307 = EDGE_CURVE ( 'NONE', #6508, #3735, #11559, .T. ) ;
#10308 = CARTESIAN_POINT ( 'NONE',  ( -16.19078112930547064, 30.00000000000008882, 73.23154106273422315 ) ) ;
#10309 = VERTEX_POINT ( 'NONE', #8673 ) ;
#10310 = CARTESIAN_POINT ( 'NONE',  ( 0.000000000000000000, 265.0000000000000000, 0.000000000000000000 ) ) ;
#10311 = CARTESIAN_POINT ( 'NONE',  ( 145.0000000000011369, 225.0000000000000853, 25.00000000000000000 ) ) ;
#10312 = DIRECTION ( 'NONE',  ( -1.000000000000000000, -0.000000000000000000, -0.000000000000000000 ) ) ;
#10313 = CARTESIAN_POINT ( 'NONE',  ( -9.777035353469207379, 42.31031047869488049, 74.36117268575515027 ) ) ;
#10314 = AXIS2_PLACEMENT_3D ( 'NONE', #4393, #4984, #12078 ) ;
#10315 = DIRECTION ( 'NONE',  ( 0.000000000000000000, 1.000000000000000000, 0.000000000000000000 ) ) ;
#10316 = CARTESIAN_POINT ( 'NONE',  ( -5.970153145843347347E-16, 111.7500000000000000, -3.250000000000000444 ) ) ;
#10317 = CARTESIAN_POINT ( 'NONE',  ( 3.202269328900650969, 15.65019529770482443, 74.93294739197928322 ) ) ;
#10318 = FACE_OUTER_BOUND ( 'NONE', #6154, .T. ) ;
#10319 = ORIENTED_EDGE ( 'NONE', *, *, #639, .F. ) ;
#10320 = CARTESIAN_POINT ( 'NONE',  ( 0.000000000000000000, 87.00000000000000000, 30.00000000000000000 ) ) ;
#10321 = FACE_OUTER_BOUND ( 'NONE', #806, .T. ) ;
#10322 = CARTESIAN_POINT ( 'NONE',  ( 11.80921887069467324, 30.00000000000008882, 80.00000000000000000 ) ) ;
#10323 = EDGE_LOOP ( 'NONE', ( #10115, #8740, #3867, #3800 ) ) ;
#10324 = EDGE_CURVE ( 'NONE', #10014, #10191, #6063, .T. ) ;
#10325 = CARTESIAN_POINT ( 'NONE',  ( 27.30107202361637775, 86.87046582918780757, 12.43589427268144831 ) ) ;
#10326 = EDGE_CURVE ( 'NONE', #10848, #3002, #9364, .T. ) ;
#10327 = CARTESIAN_POINT ( 'NONE',  ( -14.19078112930533209, 29.75000000000008882, 79.50000000000000000 ) ) ;
#10328 = VECTOR ( 'NONE', #9430, 1000.000000000000000 ) ;
#10329 = ORIENTED_EDGE ( 'NONE', *, *, #1622, .F. ) ;
#10330 = DIRECTION ( 'NONE',  ( 0.000000000000000000, 0.000000000000000000, 1.000000000000000000 ) ) ;
#10331 = EDGE_LOOP ( 'NONE', ( #5078, #3020, #11481, #10692, #9094 ) ) ;
#10332 = DIRECTION ( 'NONE',  ( -0.000000000000000000, -1.000000000000000000, -0.000000000000000000 ) ) ;
#10333 = AXIS2_PLACEMENT_3D ( 'NONE', #12098, #5424, #11219 ) ;
#10334 = LINE ( 'NONE', #12348, #8207 ) ;
#10335 = ORIENTED_EDGE ( 'NONE', *, *, #4479, .F. ) ;
#10336 = CARTESIAN_POINT ( 'NONE',  ( 0.000000000000000000, 109.0000000000000000, 3.399999999999999911 ) ) ;
#10337 = COLOUR_RGB ( '', 0.09019608, 0.27058824, 0.51372549) ;
#10338 = ORIENTED_EDGE ( 'NONE', *, *, #6254, .T. ) ;
#10339 = EDGE_CURVE ( 'NONE', #9969, #10169, #6981, .T. ) ;
#10340 = ADVANCED_FACE ( 'NONE', ( #11624 ), #135, .F. ) ;
#10341 =( NAMED_UNIT ( * ) SI_UNIT ( $, .STERADIAN. ) SOLID_ANGLE_UNIT ( ) );
#10342 = CARTESIAN_POINT ( 'NONE',  ( 0.000000000000000000, 127.0000000000000000, 0.000000000000000000 ) ) ;
#10343 = PLANE ( 'NONE',  #3621 ) ;
#10344 = DIRECTION ( 'NONE',  ( 0.000000000000000000, 0.5000000000000009992, 0.8660254037844380415 ) ) ;
#10345 = ORIENTED_EDGE ( 'NONE', *, *, #844, .T. ) ;
#10346 = CARTESIAN_POINT ( 'NONE',  ( -2.708734124999999882, 111.9999999986343937, 1.121994411437818862 ) ) ;
#10347 = EDGE_CURVE ( 'NONE', #8527, #44, #9791, .T. ) ;
#10348 = DIRECTION ( 'NONE',  ( 0.000000000000000000, 1.000000000000000000, 0.000000000000000000 ) ) ;
#10349 = VECTOR ( 'NONE', #12036, 1000.000000000000000 ) ;
#10350 = APPLICATION_CONTEXT ( 'automotive_design' ) ;
#10351 = ORIENTED_EDGE ( 'NONE', *, *, #8093, .T. ) ;
#10352 = EDGE_CURVE ( 'NONE', #737, #10899, #8959, .T. ) ;
#10353 = DIRECTION ( 'NONE',  ( -0.000000000000000000, 1.000000000000000000, -0.000000000000000000 ) ) ;
#10354 = EDGE_CURVE ( 'NONE', #9385, #9034, #7920, .T. ) ;
#10355 = DIRECTION ( 'NONE',  ( 0.000000000000000000, 0.000000000000000000, 1.000000000000000000 ) ) ;
#10356 = ORIENTED_EDGE ( 'NONE', *, *, #1751, .F. ) ;
#10357 = FACE_OUTER_BOUND ( 'NONE', #1503, .T. ) ;
#10358 = DIRECTION ( 'NONE',  ( -0.5000000000000006661, -0.8660254037844383745, 0.000000000000000000 ) ) ;
#10359 = AXIS2_PLACEMENT_3D ( 'NONE', #10810, #400, #7880 ) ;
#10360 = ORIENTED_EDGE ( 'NONE', *, *, #11584, .T. ) ;
#10361 = TOROIDAL_SURFACE ( 'NONE', #11766, 2.700000000000000622, 0.2000000000000000111 ) ;
#10362 = AXIS2_PLACEMENT_3D ( 'NONE', #5465, #12263, #6642 ) ;
#10363 = FACE_OUTER_BOUND ( 'NONE', #9766, .T. ) ;
#10364 = CARTESIAN_POINT ( 'NONE',  ( 21.00000000000000355, 0.000000000000000000, 0.000000000000000000 ) ) ;
#10365 = CARTESIAN_POINT ( 'NONE',  ( 1.121994411437818862, 110.7499999986343937, 2.708734124999999882 ) ) ;
#10366 = DIRECTION ( 'NONE',  ( 0.000000000000000000, 0.000000000000000000, 1.000000000000000000 ) ) ;
#10367 = ORIENTED_EDGE ( 'NONE', *, *, #4577, .F. ) ;
#10368 = CIRCLE ( 'NONE', #9568, 5.000000000000004441 ) ;
#10369 = AXIS2_PLACEMENT_3D ( 'NONE', #830, #9288, #12300 ) ;
#10370 = CARTESIAN_POINT ( 'NONE',  ( 29.48150359603894088, 275.0000000000000000, -121.4736224277384053 ) ) ;
#10371 = ORIENTED_EDGE ( 'NONE', *, *, #10472, .F. ) ;
#10372 = AXIS2_PLACEMENT_3D ( 'NONE', #4182, #10850, #2313 ) ;
#10373 = CARTESIAN_POINT ( 'NONE',  ( -12.32411137850302119, 23.28349364905396612, 80.00000000000000000 ) ) ;
#10374 = FACE_OUTER_BOUND ( 'NONE', #5235, .T. ) ;
#10375 = AXIS2_PLACEMENT_3D ( 'NONE', #11143, #2601, #1668 ) ;
#10376 = DIRECTION ( 'NONE',  ( 0.000000000000000000, 1.000000000000000000, 0.000000000000000000 ) ) ;
#10377 = FACE_OUTER_BOUND ( 'NONE', #3165, .T. ) ;
#10378 = CARTESIAN_POINT ( 'NONE',  ( 125.0000000000009663, 42.92893218813456713, -20.00000000000000000 ) ) ;
#10379 = EDGE_CURVE ( 'NONE', #11969, #5385, #2016, .T. ) ;
#10380 = ADVANCED_FACE ( 'NONE', ( #7685 ), #1147, .F. ) ;
#10381 = VECTOR ( 'NONE', #1539, 1000.000000000000000 ) ;
#10382 = VECTOR ( 'NONE', #6645, 1000.000000000000000 ) ;
#10383 = UNCERTAINTY_MEASURE_WITH_UNIT (LENGTH_MEASURE( 1.000000000000000082E-05 ), #463, 'distance_accuracy_value', 'NONE');
#10384 = EDGE_CURVE ( 'NONE', #5570, #6190, #8733, .T. ) ;
#10385 = CARTESIAN_POINT ( 'NONE',  ( 69.52686081653675387, 40.33415354502060524, -28.12499999996316546 ) ) ;
#10386 = CARTESIAN_POINT ( 'NONE',  ( -14.19078112930532853, 30.25000000000008882, 79.50000000000000000 ) ) ;
#10387 = ORIENTED_EDGE ( 'NONE', *, *, #3141, .T. ) ;
#10388 = DIRECTION ( 'NONE',  ( -0.000000000000000000, -0.000000000000000000, 1.000000000000000000 ) ) ;
#10389 = DIRECTION ( 'NONE',  ( -3.469446951953613203E-16, 0.000000000000000000, -1.000000000000000000 ) ) ;
#10390 = FACE_OUTER_BOUND ( 'NONE', #501, .T. ) ;
#10391 = VERTEX_POINT ( 'NONE', #261 ) ;
#10392 = CARTESIAN_POINT ( 'NONE',  ( 0.000000000000000000, 340.0000000000000000, -59.99999999999999289 ) ) ;
#10393 = DIRECTION ( 'NONE',  ( -1.000000000000000000, 0.000000000000000000, -0.000000000000000000 ) ) ;
#10394 = VECTOR ( 'NONE', #9738, 1000.000000000000000 ) ;
#10395 = EDGE_LOOP ( 'NONE', ( #2676, #8901, #3391, #8601 ) ) ;
#10396 = DIRECTION ( 'NONE',  ( 1.000000000000000000, 0.000000000000000000, 0.000000000000000000 ) ) ;
#10397 = VERTEX_POINT ( 'NONE', #6995 ) ;
#10398 = AXIS2_PLACEMENT_3D ( 'NONE', #4796, #4107, #4050 ) ;
#10399 = CARTESIAN_POINT ( 'NONE',  ( 11.80681480225048752, 29.75000000000018474, 80.00000000000000000 ) ) ;
#10400 = DIRECTION ( 'NONE',  ( 0.000000000000000000, -0.4999999999999974465, -0.8660254037844401509 ) ) ;
#10401 = ORIENTED_EDGE ( 'NONE', *, *, #5151, .F. ) ;
#10402 = CARTESIAN_POINT ( 'NONE',  ( 1.224646799147353533E-14, 265.0000000000000000, -100.0000000000000284 ) ) ;
#10403 = CARTESIAN_POINT ( 'NONE',  ( 150.0000000000010516, 15.00000000000008704, -22.92893218813451384 ) ) ;
#10404 = VERTEX_POINT ( 'NONE', #3075 ) ;
#10405 = DIRECTION ( 'NONE',  ( 1.000000000000000000, 0.000000000000000000, 0.000000000000000000 ) ) ;
#10406 = CYLINDRICAL_SURFACE ( 'NONE', #8228, 2.500000000000000444 ) ;
#10407 = DIRECTION ( 'NONE',  ( -0.000000000000000000, -0.000000000000000000, 1.000000000000000000 ) ) ;
#10408 = FACE_OUTER_BOUND ( 'NONE', #9594, .T. ) ;
#10409 = EDGE_CURVE ( 'NONE', #9640, #12119, #6878, .T. ) ;
#10410 = ORIENTED_EDGE ( 'NONE', *, *, #2470, .T. ) ;
#10411 = CARTESIAN_POINT ( 'NONE',  ( 1.121994411437819084, 114.3749999986344221, -2.708734124999999437 ) ) ;
#10412 = CIRCLE ( 'NONE', #465, 70.00000000000001421 ) ;
#10413 = CARTESIAN_POINT ( 'NONE',  ( 25.00000000000000000, 445.0000000000000568, -90.00000000000000000 ) ) ;
#10414 = EDGE_CURVE ( 'NONE', #65, #5951, #2140, .T. ) ;
#10415 = ORIENTED_EDGE ( 'NONE', *, *, #4877, .T. ) ;
#10416 = LINE ( 'NONE', #10603, #2983 ) ;
#10417 = CARTESIAN_POINT ( 'NONE',  ( 69.65097664248530407, 42.56552300069557049, 27.81636932325739409 ) ) ;
#10418 = ORIENTED_EDGE ( 'NONE', *, *, #2734, .F. ) ;
#10419 = PLANE ( 'NONE',  #4268 ) ;
#10420 = CARTESIAN_POINT ( 'NONE',  ( 72.32585155008058564, 45.16148467125184851, 19.87486525338015042 ) ) ;
#10421 = CIRCLE ( 'NONE', #5060, 4.999999999999996447 ) ;
#10422 = ORIENTED_EDGE ( 'NONE', *, *, #1137, .F. ) ;
#10423 = PLANE ( 'NONE',  #3123 ) ;
#10424 = CARTESIAN_POINT ( 'NONE',  ( 82.90657655638969459, 285.0000000000000568, 79.06642500897268633 ) ) ;
#10425 = APPLICATION_CONTEXT ( 'automotive_design' ) ;
#10426 = LINE ( 'NONE', #10491, #1599 ) ;
#10427 = ADVANCED_FACE ( 'NONE', ( #72, #6004 ), #2951, .F. ) ;
#10428 = CARTESIAN_POINT ( 'NONE',  ( 32.05000697088088657, 85.26794919243110371, 9.660254037844429931 ) ) ;
#10429 = ORIENTED_EDGE ( 'NONE', *, *, #2513, .F. ) ;
#10430 = ADVANCED_FACE ( 'NONE', ( #2195 ), #1265, .F. ) ;
#10431 =( NAMED_UNIT ( * ) SI_UNIT ( $, .STERADIAN. ) SOLID_ANGLE_UNIT ( ) );
#10432 = VECTOR ( 'NONE', #11428, 1000.000000000000000 ) ;
#10433 = CIRCLE ( 'NONE', #2873, 80.00000000000001421 ) ;
#10434 = ORIENTED_EDGE ( 'NONE', *, *, #6196, .F. ) ;
#10435 = DIRECTION ( 'NONE',  ( 0.000000000000000000, 1.000000000000000000, 0.000000000000000000 ) ) ;
#10436 = DIRECTION ( 'NONE',  ( 0.000000000000000000, 0.000000000000000000, -1.000000000000000000 ) ) ;
#10437 = ORIENTED_EDGE ( 'NONE', *, *, #2273, .F. ) ;
#10438 = DIRECTION ( 'NONE',  ( 0.000000000000000000, 1.000000000000000000, 0.000000000000000000 ) ) ;
#10439 = DIRECTION ( 'NONE',  ( 0.5000000000000066613, 0.8660254037844347108, 0.000000000000000000 ) ) ;
#10440 = CARTESIAN_POINT ( 'NONE',  ( -33.79339916392899568, 75.30908861350523864, 7.588998470350058589 ) ) ;
#10441 = DIRECTION ( 'NONE',  ( -0.8660254037844408170, 0.4999999999999961697, -0.000000000000000000 ) ) ;
#10442 = EDGE_LOOP ( 'NONE', ( #7661, #1424, #4959, #5911, #1033 ) ) ;
#10443 = AXIS2_PLACEMENT_3D ( 'NONE', #9536, #777, #4508 ) ;
#10444 =( LENGTH_UNIT ( ) NAMED_UNIT ( * ) SI_UNIT ( .MILLI., .METRE. ) );
#10445 = VECTOR ( 'NONE', #3425, 1000.000000000000000 ) ;
#10446 = CARTESIAN_POINT ( 'NONE',  ( 76.56943592554333122, 44.74351910189555070, -21.58906638518922705 ) ) ;
#10447 = VECTOR ( 'NONE', #5804, 1000.000000000000114 ) ;
#10448 = FILL_AREA_STYLE_COLOUR ( '', #719 ) ;
#10449 = ORIENTED_EDGE ( 'NONE', *, *, #4668, .T. ) ;
#10450 = LINE ( 'NONE', #11644, #4851 ) ;
#10451 = EDGE_CURVE ( 'NONE', #4547, #12062, #1643, .T. ) ;
#10452 = CARTESIAN_POINT ( 'NONE',  ( 1.346194077712578041, 112.8125000000000000, -3.249999999999981792 ) ) ;
#10453 = CARTESIAN_POINT ( 'NONE',  ( 76.19870213673728188, 15.49246197672877834, -22.18755841417196351 ) ) ;
#10454 = ORIENTED_EDGE ( 'NONE', *, *, #4341, .F. ) ;
#10455 = EDGE_CURVE ( 'NONE', #3552, #9442, #11683, .T. ) ;
#10456 = DIRECTION ( 'NONE',  ( -0.000000000000000000, -1.000000000000000000, -0.000000000000000000 ) ) ;
#10457 = ADVANCED_FACE ( 'NONE', ( #11045 ), #2507, .F. ) ;
#10458 = PRODUCT ( 'socket head cap screw_iso_ISO 4762 M5 x 16 - 16N', 'socket head cap screw_iso_ISO 4762 M5 x 16 - 16N', '', ( #12352 ) ) ;
#10459 = DIRECTION ( 'NONE',  ( 0.000000000000000000, -1.000000000000000000, 0.000000000000000000 ) ) ;
#10460 = AXIS2_PLACEMENT_3D ( 'NONE', #319, #1020, #10547 ) ;
#10461 = ORIENTED_EDGE ( 'NONE', *, *, #2215, .T. ) ;
#10462 = DIRECTION ( 'NONE',  ( 0.000000000000000000, 0.000000000000000000, 1.000000000000000000 ) ) ;
#10463 =( BOUNDED_SURFACE ( )  B_SPLINE_SURFACE ( 3, 2, ( 
 ( #5985, #9771, #114 ),
 ( #3989, #10776, #1246 ),
 ( #5054, #10593, #7663 ),
 ( #8834, #6045, #9830 ) ),
 .UNSPECIFIED., .F., .F., .F. ) 
 B_SPLINE_SURFACE_WITH_KNOTS ( ( 4, 4 ),
 ( 3, 3 ),
 ( 5.137468306293111020, 5.139829129961272614 ),
 ( 0.7666061298070568908, 1.000000000000000000 ),
 .UNSPECIFIED. ) 
 GEOMETRIC_REPRESENTATION_ITEM ( )  RATIONAL_B_SPLINE_SURFACE ( (
 ( 0.9369318869591325427, 0.9588653738936703252, 1.000000000000000000),
 ( 0.9369993130727707342, 0.9589093509185182551, 1.000000000000000000),
 ( 0.9370666800230418314, 0.9589532893555146043, 1.000000000000000000),
 ( 0.9371339877439250898, 0.9589971891615989286, 1.000000000000000000) ) ) 
 REPRESENTATION_ITEM ( '' )  SURFACE ( )  );
#10464 = CIRCLE ( 'NONE', #5101, 72.00000000000002842 ) ;
#10465 = VECTOR ( 'NONE', #11283, 1000.000000000000000 ) ;
#10466 = EDGE_LOOP ( 'NONE', ( #10755, #3315 ) ) ;
#10467 = CARTESIAN_POINT ( 'NONE',  ( 2.979367062500000163, 110.1562499993171969, 0.000000000000000000 ) ) ;
#10468 = FACE_OUTER_BOUND ( 'NONE', #5853, .T. ) ;
#10469 = ORIENTED_EDGE ( 'NONE', *, *, #2441, .T. ) ;
#10470 = VECTOR ( 'NONE', #11864, 1000.000000000000000 ) ;
#10471 = CARTESIAN_POINT ( 'NONE',  ( 30.83210227225915290, 77.00000000000000000, -6.426308247889123137 ) ) ;
#10472 = EDGE_CURVE ( 'NONE', #11969, #12341, #8226, .T. ) ;
#10473 = FACE_OUTER_BOUND ( 'NONE', #11965, .T. ) ;
#10474 = ORIENTED_EDGE ( 'NONE', *, *, #2540, .T. ) ;
#10475 = APPLICATION_PROTOCOL_DEFINITION ( 'draft international standard', 'automotive_design', 1998, #10425 ) ;
#10476 = CARTESIAN_POINT ( 'NONE',  ( 0.000000000000000000, 275.0000000000000000, 0.000000000000000000 ) ) ;
#10477 = FACE_OUTER_BOUND ( 'NONE', #11099, .T. ) ;
#10478 = CARTESIAN_POINT ( 'NONE',  ( -28.72281323269012887, 87.00000000000000000, -8.660254037844435260 ) ) ;
#10479 = EDGE_LOOP ( 'NONE', ( #5293, #9212 ) ) ;
#10480 = CARTESIAN_POINT ( 'NONE',  ( -1.915364268218909594, 111.1874999986344079, -1.915364268218908927 ) ) ;
#10481 = VECTOR ( 'NONE', #12004, 1000.000000000000000 ) ;
#10482 = EDGE_LOOP ( 'NONE', ( #3939, #10474, #6565, #3112 ) ) ;
#10483 = DIRECTION ( 'NONE',  ( -0.8660254037844398178, -0.4999999999999977796, 0.000000000000000000 ) ) ;
#10484 = CARTESIAN_POINT ( 'NONE',  ( -8.000000000000000000, 165.0000000000000000, 5.999999999999998224 ) ) ;
#10485 = ORIENTED_EDGE ( 'NONE', *, *, #6930, .F. ) ;
#10486 = DIRECTION ( 'NONE',  ( 0.000000000000000000, -0.5000000000000009992, -0.8660254037844380415 ) ) ;
#10487 = VERTEX_POINT ( 'NONE', #10093 ) ;
#10488 = CARTESIAN_POINT ( 'NONE',  ( -31.74999999999995737, 0.000000000000000000, 4.250000000000000000 ) ) ;
#10489 = PLANE ( 'NONE',  #410 ) ;
#10490 = ADVANCED_FACE ( 'NONE', ( #2375 ), #2564, .F. ) ;
#10491 = CARTESIAN_POINT ( 'NONE',  ( 25.00000000000000000, 445.0000000000000568, -88.00000000000000000 ) ) ;
#10492 = CARTESIAN_POINT ( 'NONE',  ( -2.298097038856279806, 110.6250000000000000, -2.298097038856279362 ) ) ;
#10493 = VECTOR ( 'NONE', #7244, 1000.000000000000000 ) ;
#10494 = EDGE_CURVE ( 'NONE', #9831, #7679, #5005, .T. ) ;
#10495 = CARTESIAN_POINT ( 'NONE',  ( 2.708734124999999882, 114.5624999986344079, 0.000000000000000000 ) ) ;
#10496 = ORIENTED_EDGE ( 'NONE', *, *, #5403, .T. ) ;
#10497 = EDGE_LOOP ( 'NONE', ( #10329, #9327, #3096, #1019 ) ) ;
#10498 = CARTESIAN_POINT ( 'NONE',  ( 0.000000000000000000, 5.000000000000129674, 0.000000000000000000 ) ) ;
#10499 = DIRECTION ( 'NONE',  ( -0.8660254037844383745, 0.5000000000000006661, 0.000000000000000000 ) ) ;
#10500 = ORIENTED_EDGE ( 'NONE', *, *, #10893, .T. ) ;
#10501 = CARTESIAN_POINT ( 'NONE',  ( 10.19254911989241386, 23.71650635094626836, 79.50000000000000000 ) ) ;
#10502 = DIRECTION ( 'NONE',  ( 0.000000000000000000, 1.000000000000000000, 0.000000000000000000 ) ) ;
#10503 = CARTESIAN_POINT ( 'NONE',  ( -0.9407811293054709756, 43.00000000000008527, 79.50000000000000000 ) ) ;
#10504 = CARTESIAN_POINT ( 'NONE',  ( 0.000000000000000000, 115.0000000000000000, 0.000000000000000000 ) ) ;
#10505 = ADVANCED_FACE ( 'NONE', ( #9978 ), #635, .T. ) ;
#10506 = VERTEX_POINT ( 'NONE', #8041 ) ;
#10507 = DIRECTION ( 'NONE',  ( 1.000000000000000000, 0.000000000000000000, 0.000000000000000000 ) ) ;
#10508 = EDGE_CURVE ( 'NONE', #5250, #10877, #5253, .T. ) ;
#10509 = CARTESIAN_POINT ( 'NONE',  ( 71.17928254424892032, 43.30619889802275679, -23.82724229592531273 ) ) ;
#10510 =( NAMED_UNIT ( * ) SI_UNIT ( $, .STERADIAN. ) SOLID_ANGLE_UNIT ( ) );
#10511 = CIRCLE ( 'NONE', #773, 17.00000000000000000 ) ;
#10512 = EDGE_CURVE ( 'NONE', #1340, #11798, #3380, .T. ) ;
#10513 = EDGE_CURVE ( 'NONE', #2786, #8835, #7310, .T. ) ;
#10514 = DIRECTION ( 'NONE',  ( -0.000000000000000000, -0.000000000000000000, 1.000000000000000000 ) ) ;
#10515 = PLANE ( 'NONE',  #6007 ) ;
#10516 = CARTESIAN_POINT ( 'NONE',  ( 0.000000000000000000, 2.357898499370431722, -2.818925648462311528E-15 ) ) ;
#10517 = CARTESIAN_POINT ( 'NONE',  ( 5.525725221640672480, 41.13333024919784719, 79.50000000000000000 ) ) ;
#10518 = ORIENTED_EDGE ( 'NONE', *, *, #91, .F. ) ;
#10519 = FACE_OUTER_BOUND ( 'NONE', #10479, .T. ) ;
#10520 = CYLINDRICAL_SURFACE ( 'NONE', #10737, 2.649999999999993694 ) ;
#10521 = EDGE_LOOP ( 'NONE', ( #4783, #8286, #6105, #2360, #6966 ) ) ;
#10522 = DIRECTION ( 'NONE',  ( -0.000000000000000000, -1.000000000000000000, -0.000000000000000000 ) ) ;
#10523 = ORIENTED_EDGE ( 'NONE', *, *, #9346, .F. ) ;
#10524 = DIRECTION ( 'NONE',  ( 0.000000000000000000, 0.000000000000000000, 1.000000000000000000 ) ) ;
#10525 = CARTESIAN_POINT ( 'NONE',  ( 74.19368986856427739, 40.71666413485492342, 24.96097029013992241 ) ) ;
#10526 = ORIENTED_EDGE ( 'NONE', *, *, #6349, .F. ) ;
#10527 = DIRECTION ( 'NONE',  ( -1.000000000000000000, 0.000000000000000000, 0.000000000000000000 ) ) ;
#10528 = DIRECTION ( 'NONE',  ( 0.000000000000000000, 0.000000000000000000, -1.000000000000000000 ) ) ;
#10529 = ORIENTED_EDGE ( 'NONE', *, *, #903, .T. ) ;
#10530 = DIRECTION ( 'NONE',  ( 0.000000000000000000, -1.000000000000000000, 0.000000000000000000 ) ) ;
#10531 = DIRECTION ( 'NONE',  ( -0.000000000000000000, 0.000000000000000000, 1.000000000000000000 ) ) ;
#10532 = DIRECTION ( 'NONE',  ( 0.000000000000000000, 0.000000000000000000, 1.000000000000000000 ) ) ;
#10533 = VERTEX_POINT ( 'NONE', #1327 ) ;
#10534 = CARTESIAN_POINT ( 'NONE',  ( 1.915364268218909594, 111.4374999986344079, 1.915364268218909594 ) ) ;
#10535 = FACE_OUTER_BOUND ( 'NONE', #5874, .T. ) ;
#10536 = EDGE_CURVE ( 'NONE', #875, #10397, #8767, .T. ) ;
#10537 = AXIS2_PLACEMENT_3D ( 'NONE', #3102, #5913, #4041 ) ;
#10538 = AXIS2_PLACEMENT_3D ( 'NONE', #2694, #9225, #3631 ) ;
#10539 = ORIENTED_EDGE ( 'NONE', *, *, #11516, .F. ) ;
#10540 = CARTESIAN_POINT ( 'NONE',  ( 3.250000000000000444, 110.8749999972688158, 0.000000000000000000 ) ) ;
#10541 = ADVANCED_FACE ( 'NONE', ( #7179 ), #10981, .F. ) ;
#10542 = DIRECTION ( 'NONE',  ( -0.000000000000000000, -1.000000000000000000, -0.000000000000000000 ) ) ;
#10543 = VERTEX_POINT ( 'NONE', #10038 ) ;
#10544 = CARTESIAN_POINT ( 'NONE',  ( 10.06754911989234635, 23.50000000000004974, 80.00000000000000000 ) ) ;
#10545 = PLANE ( 'NONE',  #7081 ) ;
#10546 = VERTEX_POINT ( 'NONE', #1511 ) ;
#10547 = DIRECTION ( 'NONE',  ( 0.000000000000000000, 0.000000000000000000, -1.000000000000000000 ) ) ;
#10548 = DIRECTION ( 'NONE',  ( -0.000000000000000000, 1.000000000000000000, -0.000000000000000000 ) ) ;
#10549 = CARTESIAN_POINT ( 'NONE',  ( 117.9289321881355193, 40.00000000000009237, 20.00000000000000000 ) ) ;
#10550 = CIRCLE ( 'NONE', #12161, 125.0000000000000284 ) ;
#10551 = LINE ( 'NONE', #7626, #4181 ) ;
#10552 = DIRECTION ( 'NONE',  ( -0.000000000000000000, -1.000000000000000000, -0.000000000000000000 ) ) ;
#10553 = CARTESIAN_POINT ( 'NONE',  ( -2.708734125000000326, 112.1249999986343937, -1.121994411437818195 ) ) ;
#10554 =( BOUNDED_SURFACE ( )  B_SPLINE_SURFACE ( 3, 2, ( 
 ( #1519, #8049, #9100 ),
 ( #11814, #3325, #6945 ),
 ( #1455, #3257, #7125 ),
 ( #329, #7065, #2324 ),
 ( #6131, #1391, #10923 ),
 ( #2381, #923, #10446 ),
 ( #9626, #3204, #2780 ),
 ( #1107, #5722, #7004 ),
 ( #5784, #7927, #11520 ),
 ( #2039, #8695, #9861 ),
 ( #2909, #6772, #1913 ),
 ( #5144, #11395, #7708 ),
 ( #1974, #4911, #4198 ),
 ( #2972, #4843, #9566 ),
 ( #1847, #2847, #10571 ),
 ( #5842, #10509, #94 ),
 ( #10801, #983, #8630 ),
 ( #1042, #5660, #3968 ),
 ( #8920, #390, #4715 ),
 ( #9439, #4776, #11750 ),
 ( #6648, #6587, #8567 ),
 ( #8507, #7645, #6071 ),
 ( #3911, #157, #31 ),
 ( #2261, #1336, #11332 ),
 ( #10385, #12330, #9500 ),
 ( #3778, #6713, #7581 ) ),
 .UNSPECIFIED., .F., .F., .F. ) 
 B_SPLINE_SURFACE_WITH_KNOTS ( ( 4, 2, 2, 2, 2, 2, 2, 2, 2, 2, 2, 2, 4 ),
 ( 3, 3 ),
 ( 0.006933106248791174805, 0.008937828180681107321, 0.009940189146626074446, 0.01094255011257104157, 0.01294727204446097409, 0.01394963301040593948, 0.01495199397635090660, 0.01695671590824084085, 0.01795907687418580798, 0.01896143784013077510, 0.02096615977202070935, 0.02196852073796567301, 0.02297088170391064013 ),
 ( 0.000000000000000000, 1.000000000000000000 ),
 .UNSPECIFIED. ) 
 GEOMETRIC_REPRESENTATION_ITEM ( )  RATIONAL_B_SPLINE_SURFACE ( (
 ( 1.000000000000000000, 0.7071067811865475727, 1.000000000000000000),
 ( 1.000000000000000000, 0.7129067084832356738, 1.000000000000000000),
 ( 1.000000000000000000, 0.7190912265161183425, 1.000000000000000000),
 ( 1.000000000000000000, 0.7288225095607339110, 1.000000000000000000),
 ( 1.000000000000000000, 0.7321420440090409265, 1.000000000000000000),
 ( 1.000000000000000000, 0.7389120750275461891, 1.000000000000000000),
 ( 1.000000000000000000, 0.7423805904413234291, 1.000000000000000000),
 ( 1.000000000000000000, 0.7527643000947431551, 1.000000000000000000),
 ( 1.000000000000000000, 0.7596816647252027099, 1.000000000000000000),
 ( 1.000000000000000000, 0.7698812226850976215, 1.000000000000000000),
 ( 1.000000000000000000, 0.7732515396852110978, 1.000000000000000000),
 ( 1.000000000000000000, 0.7799012531313249674, 1.000000000000000000),
 ( 1.000000000000000000, 0.7831631659391801170, 1.000000000000000000),
 ( 1.000000000000000000, 0.7925626959608614852, 1.000000000000000000),
 ( 1.000000000000000000, 0.7983806636883183927, 1.000000000000000000),
 ( 1.000000000000000000, 0.8062586255457302453, 1.000000000000000000),
 ( 1.000000000000000000, 0.8087533637821522348, 1.000000000000000000),
 ( 1.000000000000000000, 0.8133656295006947978, 1.000000000000000000),
 ( 1.000000000000000000, 0.8154682471119685250, 1.000000000000000000),
 ( 1.000000000000000000, 0.8211473929489091494, 1.000000000000000000),
 ( 1.000000000000000000, 0.8241004955462456483, 1.000000000000000000),
 ( 1.000000000000000000, 0.8271253898583996733, 1.000000000000000000),
 ( 1.000000000000000000, 0.8278923858075547537, 1.000000000000000000),
 ( 1.000000000000000000, 0.8289041354387917115, 1.000000000000000000),
 ( 1.000000000000000000, 0.8291560334507813712, 1.000000000000000000),
 ( 1.000000000000000000, 0.8291561975888499525, 1.000000000000000000) ) ) 
 REPRESENTATION_ITEM ( '' )  SURFACE ( )  );
#10555 = ORIENTED_EDGE ( 'NONE', *, *, #1345, .F. ) ;
#10556 = TOROIDAL_SURFACE ( 'NONE', #4388, 4.000000000000000000, 0.2500000000000000000 ) ;
#10557 = AXIS2_PLACEMENT_3D ( 'NONE', #2091, #10749, #8870 ) ;
#10558 = LINE ( 'NONE', #910, #3465 ) ;
#10559 = CARTESIAN_POINT ( 'NONE',  ( 8.122470672675945025, 41.76773423473973423, 74.55981757952413602 ) ) ;
#10560 = ORIENTED_EDGE ( 'NONE', *, *, #5125, .T. ) ;
#10561 = DIRECTION ( 'NONE',  ( 0.8660254037844434816, 0.4999999999999913958, 0.000000000000000000 ) ) ;
#10562 = CARTESIAN_POINT ( 'NONE',  ( 0.000000000000000000, 122.0000000000000000, 0.000000000000000000 ) ) ;
#10563 = CARTESIAN_POINT ( 'NONE',  ( -30.15809951803416666, 76.87504465863048608, 4.876683037773544172 ) ) ;
#10564 = CARTESIAN_POINT ( 'NONE',  ( 0.000000000000000000, 285.0000000000000568, -115.0000000000000284 ) ) ;
#10565 = ORIENTED_EDGE ( 'NONE', *, *, #596, .F. ) ;
#10566 = VECTOR ( 'NONE', #3195, 1000.000000000000000 ) ;
#10567 = DIRECTION ( 'NONE',  ( 0.000000000000000000, 1.000000000000000000, 0.000000000000000000 ) ) ;
#10568 = EDGE_LOOP ( 'NONE', ( #9260, #751, #1453, #5189 ) ) ;
#10569 = AXIS2_PLACEMENT_3D ( 'NONE', #11103, #502, #439 ) ;
#10570 = ADVANCED_FACE ( 'NONE', ( #7979 ), #11807, .T. ) ;
#10571 = CARTESIAN_POINT ( 'NONE',  ( 74.98307306353127899, 43.09120835303954777, -23.94359236839000360 ) ) ;
#10572 = PRESENTATION_STYLE_ASSIGNMENT (( #8696 ) ) ;
#10573 = AXIS2_PLACEMENT_3D ( 'NONE', #9959, #3431, #364 ) ;
#10574 = DIRECTION ( 'NONE',  ( 0.000000000000000000, 0.8660254037844407060, -0.4999999999999965583 ) ) ;
#10575 = B_SPLINE_CURVE_WITH_KNOTS ( 'NONE', 3,
 ( #4897, #9736, #2961, #1032, #208, #5954, #3900, #4081, #4958, #7874, #4019, #6758, #7633, #6948, #10559, #5086, #2027, #11447, #1217, #5021, #2898, #7818, #6824, #5894 ),
 .UNSPECIFIED., .F., .F.,
 ( 4, 2, 2, 2, 2, 2, 2, 2, 2, 2, 2, 4 ),
 ( 0.02230690517119256200, 0.02509601044920642052, 0.02788511572722027904, 0.02927966836622719615, 0.03067422100523411674, 0.03346332628324795444, 0.03485787892225486462, 0.03625243156126176786, 0.03904153683927557433, 0.04043608947828247757, 0.04183064211728938775, 0.04461974739530318729 ),
 .UNSPECIFIED. ) ;
#10576 = CARTESIAN_POINT ( 'NONE',  ( 143.5355339059338462, 61.46446609406724804, -25.00000000000000000 ) ) ;
#10577 = CARTESIAN_POINT ( 'NONE',  ( -0.9407811293054709756, 43.00000000000008527, 80.00000000000000000 ) ) ;
#10578 = CARTESIAN_POINT ( 'NONE',  ( 71.31012073600892620, 16.24668676079221896, -23.41524959671153638 ) ) ;
#10579 = ORIENTED_EDGE ( 'NONE', *, *, #7001, .T. ) ;
#10580 = CARTESIAN_POINT ( 'NONE',  ( -3.250000000000000444, 111.5000000000000000, 3.980102097228898231E-16 ) ) ;
#10581 = DIRECTION ( 'NONE',  ( 0.000000000000000000, 0.000000000000000000, -1.000000000000000000 ) ) ;
#10582 = VECTOR ( 'NONE', #1230, 1000.000000000000000 ) ;
#10583 = VERTEX_POINT ( 'NONE', #2318 ) ;
#10584 = CYLINDRICAL_SURFACE ( 'NONE', #2599, 125.0000000000000284 ) ;
#10585 = EDGE_CURVE ( 'NONE', #2064, #7160, #7975, .T. ) ;
#10586 = EDGE_CURVE ( 'NONE', #8667, #12030, #9093, .T. ) ;
#10587 = VERTEX_POINT ( 'NONE', #7119 ) ;
#10588 = CARTESIAN_POINT ( 'NONE',  ( 0.000000000000000000, 77.00000000000000000, 0.000000000000000000 ) ) ;
#10589 = CARTESIAN_POINT ( 'NONE',  ( 76.05694877984102220, 44.39411534459425468, 22.40616324080664157 ) ) ;
#10590 = ORIENTED_EDGE ( 'NONE', *, *, #12178, .F. ) ;
#10591 = APPLICATION_CONTEXT ( 'automotive_design' ) ;
#10592 = CARTESIAN_POINT ( 'NONE',  ( -2.298097038856279362, 111.2499999972688158, 2.298097038856279806 ) ) ;
#10593 = CARTESIAN_POINT ( 'NONE',  ( 27.55156151032568701, 86.54395234961377525, 11.88489976664085113 ) ) ;
#10594 = ORIENTED_EDGE ( 'NONE', *, *, #5321, .T. ) ;
#10595 = APPLICATION_PROTOCOL_DEFINITION ( 'draft international standard', 'automotive_design', 1998, #12278 ) ;
#10596 = DIRECTION ( 'NONE',  ( 1.000000000000000000, 0.000000000000000000, 0.000000000000000000 ) ) ;
#10597 = FACE_OUTER_BOUND ( 'NONE', #1717, .T. ) ;
#10598 = EDGE_LOOP ( 'NONE', ( #4644, #7109, #10840, #8435 ) ) ;
#10599 = CARTESIAN_POINT ( 'NONE',  ( 2.708734125000000326, 114.3124999986344079, 0.000000000000000000 ) ) ;
#10600 = CARTESIAN_POINT ( 'NONE',  ( -3.250000000000000444, 112.3124999972688016, 1.346194077712559389 ) ) ;
#10601 = VECTOR ( 'NONE', #10561, 1000.000000000000114 ) ;
#10602 = VERTEX_POINT ( 'NONE', #10916 ) ;
#10603 = CARTESIAN_POINT ( 'NONE',  ( 0.000000000000000000, 165.0000000000000000, 2.099999999999993427 ) ) ;
#10604 = CARTESIAN_POINT ( 'NONE',  ( 0.000000000000000000, 275.0000000000000000, 0.000000000000000000 ) ) ;
#10605 = ORIENTED_EDGE ( 'NONE', *, *, #4353, .F. ) ;
#10606 = DIRECTION ( 'NONE',  ( 0.000000000000000000, 0.000000000000000000, 1.000000000000000000 ) ) ;
#10607 = CARTESIAN_POINT ( 'NONE',  ( 27.33018067101282966, 87.00000000000000000, 12.37179148263486539 ) ) ;
#10608 = ORIENTED_EDGE ( 'NONE', *, *, #4879, .T. ) ;
#10609 = DIRECTION ( 'NONE',  ( 0.000000000000000000, 1.000000000000000000, 0.000000000000000000 ) ) ;
#10610 = EDGE_CURVE ( 'NONE', #686, #10506, #6183, .T. ) ;
#10611 = ADVANCED_FACE ( 'NONE', ( #570 ), #420, .T. ) ;
#10612 = DIRECTION ( 'NONE',  ( -0.000000000000000000, 0.000000000000000000, 1.000000000000000000 ) ) ;
#10613 = CARTESIAN_POINT ( 'NONE',  ( 0.000000000000000000, 0.000000000000000000, 79.50000000000000000 ) ) ;
#10614 = CARTESIAN_POINT ( 'NONE',  ( 0.000000000000000000, 75.00000000000001421, 0.000000000000000000 ) ) ;
#10615 = CARTESIAN_POINT ( 'NONE',  ( 3.122849337825750222E-15, 77.00000000000000000, 25.50000000000000000 ) ) ;
#10616 = CARTESIAN_POINT ( 'NONE',  ( -2.708734124999999882, 112.0624999986344079, 3.317242575922456639E-16 ) ) ;
#10617 = EDGE_CURVE ( 'NONE', #343, #8712, #766, .T. ) ;
#10618 = SURFACE_STYLE_USAGE ( .BOTH. , #8680 ) ;
#10619 = VERTEX_POINT ( 'NONE', #6434 ) ;
#10620 = AXIS2_PLACEMENT_3D ( 'NONE', #4216, #11894, #11830 ) ;
#10621 = CARTESIAN_POINT ( 'NONE',  ( 45.35898384862240107, 85.26794919243110371, 9.660254037844429931 ) ) ;
#10622 = DIRECTION ( 'NONE',  ( 0.000000000000000000, 1.000000000000000000, 0.000000000000000000 ) ) ;
#10623 = ORIENTED_EDGE ( 'NONE', *, *, #8044, .F. ) ;
#10624 = FACE_OUTER_BOUND ( 'NONE', #11785, .T. ) ;
#10625 = CARTESIAN_POINT ( 'NONE',  ( -3.250000000000001776, 112.4374999972688300, -1.346194077712558279 ) ) ;
#10626 = CARTESIAN_POINT ( 'NONE',  ( -30.07733313487553772, 77.00000000000709122, 4.660254037819535178 ) ) ;
#10627 = LINE ( 'NONE', #6952, #11576 ) ;
#10628 = ORIENTED_EDGE ( 'NONE', *, *, #8044, .T. ) ;
#10629 = COLOUR_RGB ( '', 0.72549020, 0.75294118, 0.79215686) ;
#10630 = AXIS2_PLACEMENT_3D ( 'NONE', #7902, #5056, #491 ) ;
#10631 = ORIENTED_EDGE ( 'NONE', *, *, #11728, .F. ) ;
#10632 = DIRECTION ( 'NONE',  ( -1.000000000000000000, 0.000000000000000000, 0.000000000000000000 ) ) ;
#10633 = DIRECTION ( 'NONE',  ( -0.000000000000000000, -1.000000000000000000, -0.000000000000000000 ) ) ;
#10634 = CARTESIAN_POINT ( 'NONE',  ( 9.942549119892305498, 36.71650635094628967, 79.50000000000000000 ) ) ;
#10635 = ORIENTED_EDGE ( 'NONE', *, *, #10414, .T. ) ;
#10636 = VECTOR ( 'NONE', #11467, 1000.000000000000000 ) ;
#10637 = LINE ( 'NONE', #10516, #12054 ) ;
#10638 = CARTESIAN_POINT ( 'NONE',  ( 70.30108951986159127, 13.82498561756345445, -26.13045860990803249 ) ) ;
#10639 = VERTEX_POINT ( 'NONE', #7491 ) ;
#10640 = CARTESIAN_POINT ( 'NONE',  ( -45.35898384862240107, 85.26794919243110371, -9.660254037844419273 ) ) ;
#10641 = LINE ( 'NONE', #40, #4357 ) ;
#10642 = EDGE_CURVE ( 'NONE', #6005, #10667, #6499, .T. ) ;
#10643 = ORIENTED_EDGE ( 'NONE', *, *, #11654, .T. ) ;
#10644 = CARTESIAN_POINT ( 'NONE',  ( 0.000000000000000000, 260.0000000000000000, 0.000000000000000000 ) ) ;
#10645 = EDGE_CURVE ( 'NONE', #6005, #11474, #10368, .T. ) ;
#10646 = CIRCLE ( 'NONE', #6067, 17.00000000000000000 ) ;
#10647 = AXIS2_PLACEMENT_3D ( 'NONE', #6319, #10863, #5262 ) ;
#10648 = ORIENTED_EDGE ( 'NONE', *, *, #6984, .T. ) ;
#10649 = DIRECTION ( 'NONE',  ( -1.000000000000000000, -0.000000000000000000, -0.000000000000000000 ) ) ;
#10650 = DIRECTION ( 'NONE',  ( -0.000000000000000000, -1.000000000000000000, -0.000000000000000000 ) ) ;
#10651 = ORIENTED_EDGE ( 'NONE', *, *, #1886, .F. ) ;
#10652 = LINE ( 'NONE', #8650, #9834 ) ;
#10653 = DIRECTION ( 'NONE',  ( -1.000000000000000000, 0.000000000000000000, 0.000000000000000000 ) ) ;
#10654 = ORIENTED_EDGE ( 'NONE', *, *, #1516, .T. ) ;
#10655 = STYLED_ITEM ( 'NONE', ( #2342 ), #4709 ) ;
#10656 = DIRECTION ( 'NONE',  ( 0.000000000000000000, 0.000000000000000000, 1.000000000000000000 ) ) ;
#10657 = DIRECTION ( 'NONE',  ( 0.000000000000000000, 1.000000000000000000, 0.000000000000000000 ) ) ;
#10658 = ADVANCED_FACE ( 'NONE', ( #4679 ), #9341, .T. ) ;
#10659 = ORIENTED_EDGE ( 'NONE', *, *, #11441, .T. ) ;
#10660 = CARTESIAN_POINT ( 'NONE',  ( 1.121994411437818862, 111.4999999986343937, 2.708734125000000326 ) ) ;
#10661 = CARTESIAN_POINT ( 'NONE',  ( 1.990051048614449116E-16, 113.1249999972688158, 3.250000000000000444 ) ) ;
#10662 = PRODUCT ( 'Clear Processing Bowl', 'Clear Processing Bowl', '', ( #7789 ) ) ;
#10663 = VECTOR ( 'NONE', #9848, 1000.000000000000114 ) ;
#10664 = EDGE_LOOP ( 'NONE', ( #9370, #10701, #3033, #12166 ) ) ;
#10665 = DIRECTION ( 'NONE',  ( -1.000000000000000000, 3.469446951953611033E-15, 0.000000000000000000 ) ) ;
#10666 = FACE_OUTER_BOUND ( 'NONE', #8926, .T. ) ;
#10667 = VERTEX_POINT ( 'NONE', #8412 ) ;
#10668 = AXIS2_PLACEMENT_3D ( 'NONE', #5421, #3604, #2785 ) ;
#10669 = DIRECTION ( 'NONE',  ( 1.000000000000000000, -0.000000000000000000, 0.000000000000000000 ) ) ;
#10670 = DIRECTION ( 'NONE',  ( -0.000000000000000000, 1.000000000000000000, -0.000000000000000000 ) ) ;
#10671 = ORIENTED_EDGE ( 'NONE', *, *, #7075, .F. ) ;
#10672 = EDGE_CURVE ( 'NONE', #7113, #10772, #8172, .T. ) ;
#10673 = ADVANCED_FACE ( 'NONE', ( #3625 ), #11171, .T. ) ;
#10674 = DIRECTION ( 'NONE',  ( 0.000000000000000000, -0.4999999999999974465, -0.8660254037844401509 ) ) ;
#10675 = CARTESIAN_POINT ( 'NONE',  ( 74.40577577445179713, 41.75081809461674709, -24.69584740025122471 ) ) ;
#10676 = DIRECTION ( 'NONE',  ( 0.000000000000000000, 0.000000000000000000, -1.000000000000000000 ) ) ;
#10677 = DIRECTION ( 'NONE',  ( 0.000000000000000000, 0.000000000000000000, 1.000000000000000000 ) ) ;
#10678 = CARTESIAN_POINT ( 'NONE',  ( 170.0000000000011369, 225.0000000000000853, -19.99999999999999645 ) ) ;
#10679 = LINE ( 'NONE', #6941, #8768 ) ;
#10680 = PRESENTATION_LAYER_ASSIGNMENT (  '', '', ( #9473 ) ) ;
#10681 = ORIENTED_EDGE ( 'NONE', *, *, #3331, .F. ) ;
#10682 = ORIENTED_EDGE ( 'NONE', *, *, #9657, .F. ) ;
#10683 = CARTESIAN_POINT ( 'NONE',  ( 170.0000000000011369, 35.00000000000004974, 20.00000000000000000 ) ) ;
#10684 = CARTESIAN_POINT ( 'NONE',  ( 0.000000000000000000, 285.0000000000000568, 0.000000000000000000 ) ) ;
#10685 = VERTEX_POINT ( 'NONE', #699 ) ;
#10686 = DIRECTION ( 'NONE',  ( 1.000000000000000000, 0.000000000000000000, 0.000000000000000000 ) ) ;
#10687 = CARTESIAN_POINT ( 'NONE',  ( 0.000000000000000000, 115.0000000000000000, 0.000000000000000000 ) ) ;
#10688 = CIRCLE ( 'NONE', #4312, 9.999999999999994671 ) ;
#10689 = LINE ( 'NONE', #8690, #5512 ) ;
#10690 = CARTESIAN_POINT ( 'NONE',  ( 2.708734125000000326, 110.3124999986344079, 0.000000000000000000 ) ) ;
#10691 = ORIENTED_EDGE ( 'NONE', *, *, #10829, .F. ) ;
#10692 = ORIENTED_EDGE ( 'NONE', *, *, #9234, .F. ) ;
#10693 = ADVANCED_FACE ( 'NONE', ( #10408 ), #7433, .T. ) ;
#10694 = DIRECTION ( 'NONE',  ( 1.224646799147352961E-16, 0.000000000000000000, -1.000000000000000000 ) ) ;
#10695 = DIRECTION ( 'NONE',  ( 0.000000000000000000, 1.000000000000000000, 0.000000000000000000 ) ) ;
#10696 = CARTESIAN_POINT ( 'NONE',  ( 0.000000000000000000, 0.000000000000000000, 0.000000000000000000 ) ) ;
#10697 = CARTESIAN_POINT ( 'NONE',  ( 145.0000000000011369, 225.0000000000000853, 20.00000000000000000 ) ) ;
#10698 = CARTESIAN_POINT ( 'NONE',  ( 76.75496552995652166, 15.16338392435726945, -21.27808286176472308 ) ) ;
#10699 = DIRECTION ( 'NONE',  ( 0.000000000000000000, 0.000000000000000000, -1.000000000000000000 ) ) ;
#10700 = CARTESIAN_POINT ( 'NONE',  ( 1.915364268218909594, 110.4374999986344079, 1.915364268218909594 ) ) ;
#10701 = ORIENTED_EDGE ( 'NONE', *, *, #2085, .F. ) ;
#10702 = FACE_OUTER_BOUND ( 'NONE', #6501, .T. ) ;
#10703 = EDGE_CURVE ( 'NONE', #1747, #4020, #10286, .T. ) ;
#10704 = AXIS2_PLACEMENT_3D ( 'NONE', #1805, #3984, #9394 ) ;
#10705 =( GEOMETRIC_REPRESENTATION_CONTEXT ( 3 ) GLOBAL_UNCERTAINTY_ASSIGNED_CONTEXT ( ( #8504 ) ) GLOBAL_UNIT_ASSIGNED_CONTEXT ( ( #6756, #4893, #10431 ) ) REPRESENTATION_CONTEXT ( 'NONE', 'WORKASPACE' ) );
#10706 = VERTEX_POINT ( 'NONE', #1755 ) ;
#10707 = EDGE_CURVE ( 'NONE', #5644, #6060, #11302, .T. ) ;
#10708 = CARTESIAN_POINT ( 'NONE',  ( -31.26438337082141672, 85.29075299833054657, -9.699751388268188279 ) ) ;
#10709 = CARTESIAN_POINT ( 'NONE',  ( 89.80805993797383735, 285.0000000000000568, 71.82974571984303225 ) ) ;
#10710 = EDGE_LOOP ( 'NONE', ( #1270, #9460, #9601, #4854 ) ) ;
#10711 = ADVANCED_FACE ( 'NONE', ( #1870 ), #2743, .T. ) ;
#10712 = CARTESIAN_POINT ( 'NONE',  ( 0.000000000000000000, -2.357898499370432166, 3.035766082959412415E-15 ) ) ;
#10713 = DIRECTION ( 'NONE',  ( 0.000000000000000000, 1.000000000000000000, 0.000000000000000000 ) ) ;
#10714 = ORIENTED_EDGE ( 'NONE', *, *, #9128, .F. ) ;
#10715 = DIRECTION ( 'NONE',  ( -0.000000000000000000, -1.000000000000000000, -0.000000000000000000 ) ) ;
#10716 = CARTESIAN_POINT ( 'NONE',  ( 0.000000000000000000, 285.0000000000000568, 0.000000000000000000 ) ) ;
#10717 = MECHANICAL_DESIGN_GEOMETRIC_PRESENTATION_REPRESENTATION (  '', ( #10113 ), #11329 ) ;
#10718 = VERTEX_POINT ( 'NONE', #5626 ) ;
#10719 = CARTESIAN_POINT ( 'NONE',  ( 2.708734125000000326, 111.3749999986344221, 1.121994411437818862 ) ) ;
#10720 = CARTESIAN_POINT ( 'NONE',  ( -1.346194077712559389, 114.1874999972688016, 3.250000000000000444 ) ) ;
#10721 = ORIENTED_EDGE ( 'NONE', *, *, #4176, .T. ) ;
#10722 = ADVANCED_FACE ( 'NONE', ( #8470 ), #884, .T. ) ;
#10723 = EDGE_CURVE ( 'NONE', #2576, #11144, #7903, .T. ) ;
#10724 = CYLINDRICAL_SURFACE ( 'NONE', #10305, 25.50000000000000000 ) ;
#10725 = DIRECTION ( 'NONE',  ( 0.000000000000000000, -0.000000000000000000, 1.000000000000000000 ) ) ;
#10726 = EDGE_LOOP ( 'NONE', ( #12023, #6687, #3360 ) ) ;
#10727 = PLANE ( 'NONE',  #11176 ) ;
#10728 = FACE_OUTER_BOUND ( 'NONE', #5813, .T. ) ;
#10729 = ORIENTED_EDGE ( 'NONE', *, *, #8491, .T. ) ;
#10730 = DIRECTION ( 'NONE',  ( -1.000000000000000000, -0.000000000000000000, -0.000000000000000000 ) ) ;
#10731 = DIRECTION ( 'NONE',  ( -1.000000000000000000, 0.000000000000000000, 0.000000000000000000 ) ) ;
#10732 = CARTESIAN_POINT ( 'NONE',  ( -34.80930551369991122, 75.84619333735180646, 7.994103450571739877 ) ) ;
#10733 = MECHANICAL_DESIGN_GEOMETRIC_PRESENTATION_REPRESENTATION (  '', ( #7865 ), #1585 ) ;
#10734 = ORIENTED_EDGE ( 'NONE', *, *, #3004, .F. ) ;
#10735 = PLANE ( 'NONE',  #6768 ) ;
#10736 = CARTESIAN_POINT ( 'NONE',  ( 1.915364268218908705, 112.4374999986344079, -1.915364268218909594 ) ) ;
#10737 = AXIS2_PLACEMENT_3D ( 'NONE', #9510, #7717, #1049 ) ;
#10738 = AXIS2_PLACEMENT_3D ( 'NONE', #2943, #6743, #9599 ) ;
#10739 = ADVANCED_FACE ( 'NONE', ( #8290, #3564 ), #9285, .F. ) ;
#10740 = VERTEX_POINT ( 'NONE', #305 ) ;
#10741 = LINE ( 'NONE', #3389, #4278 ) ;
#10742 = VERTEX_POINT ( 'NONE', #8837 ) ;
#10743 = PRODUCT_DEFINITION_CONTEXT ( 'detailed design', #6138, 'design' ) ;
#10744 = CARTESIAN_POINT ( 'NONE',  ( 30.07733313487553772, 77.00000000000709122, -4.660254037819535178 ) ) ;
#10745 = CARTESIAN_POINT ( 'NONE',  ( 0.000000000000000000, 63.00000000000000000, -57.08203932499371547 ) ) ;
#10746 = VERTEX_POINT ( 'NONE', #2938 ) ;
#10747 = CARTESIAN_POINT ( 'NONE',  ( 2.020667218593133416E-14, 63.00000000000000000, 70.00000000000000000 ) ) ;
#10748 = CIRCLE ( 'NONE', #5379, 30.00000000000000355 ) ;
#10749 = DIRECTION ( 'NONE',  ( 0.000000000000000000, 1.000000000000000000, 0.000000000000000000 ) ) ;
#10750 = DIRECTION ( 'NONE',  ( -0.000000000000000000, 1.000000000000000000, -0.000000000000000000 ) ) ;
#10751 = AXIS2_PLACEMENT_3D ( 'NONE', #9567, #3846, #9441 ) ;
#10752 = CARTESIAN_POINT ( 'NONE',  ( 0.000000000000000000, 65.00000000000000000, -57.08203932499371547 ) ) ;
#10753 = VECTOR ( 'NONE', #1085, 1000.000000000000000 ) ;
#10754 =( NAMED_UNIT ( * ) PLANE_ANGLE_UNIT ( ) SI_UNIT ( $, .RADIAN. ) );
#10755 = ORIENTED_EDGE ( 'NONE', *, *, #89, .T. ) ;
#10756 = CIRCLE ( 'NONE', #4997, 10.49999999999999822 ) ;
#10757 = CYLINDRICAL_SURFACE ( 'NONE', #3306, 75.00000000000001421 ) ;
#10758 = CARTESIAN_POINT ( 'NONE',  ( 5.200000000000002842, 3.306546357697854226E-16, 2.700000000000000622 ) ) ;
#10759 = CARTESIAN_POINT ( 'NONE',  ( -12.57411137850301763, 23.71650635094618664, 79.50000000000000000 ) ) ;
#10760 = CARTESIAN_POINT ( 'NONE',  ( 0.000000000000000000, 20.00000000000009237, 20.00000000000000000 ) ) ;
#10761 = VECTOR ( 'NONE', #3889, 1000.000000000000000 ) ;
#10762 = DIRECTION ( 'NONE',  ( 0.000000000000000000, -1.000000000000000000, 0.000000000000000000 ) ) ;
#10763 =( GEOMETRIC_REPRESENTATION_CONTEXT ( 3 ) GLOBAL_UNCERTAINTY_ASSIGNED_CONTEXT ( ( #2397 ) ) GLOBAL_UNIT_ASSIGNED_CONTEXT ( ( #218, #6833, #2100 ) ) REPRESENTATION_CONTEXT ( 'NONE', 'WORKASPACE' ) );
#10764 = FACE_OUTER_BOUND ( 'NONE', #6875, .T. ) ;
#10765 = EDGE_CURVE ( 'NONE', #11680, #9447, #11377, .T. ) ;
#10766 = EDGE_CURVE ( 'NONE', #1112, #4135, #3214, .T. ) ;
#10767 = CARTESIAN_POINT ( 'NONE',  ( 1.121994411437818862, 113.4999999986344079, 2.708734125000000326 ) ) ;
#10768 = VERTEX_POINT ( 'NONE', #6922 ) ;
#10769 = CARTESIAN_POINT ( 'NONE',  ( 0.000000000000000000, 265.0000000000000000, 95.00000000000002842 ) ) ;
#10770 = EDGE_CURVE ( 'NONE', #10718, #10032, #3935, .T. ) ;
#10771 = AXIS2_PLACEMENT_3D ( 'NONE', #10716, #2869, #7669 ) ;
#10772 = VERTEX_POINT ( 'NONE', #10478 ) ;
#10773 = FACE_OUTER_BOUND ( 'NONE', #742, .T. ) ;
#10774 = EDGE_LOOP ( 'NONE', ( #11630, #8628, #8309, #5635, #10172 ) ) ;
#10775 = PLANE ( 'NONE',  #9438 ) ;
#10776 = CARTESIAN_POINT ( 'NONE',  ( 27.56105762898382139, 86.58728811733513453, 11.86287969473300308 ) ) ;
#10777 = EDGE_LOOP ( 'NONE', ( #6160, #7870, #9055, #11319 ) ) ;
#10778 = CARTESIAN_POINT ( 'NONE',  ( -13.00000000000000178, 216.0365690573663926, 7.483314773547879106 ) ) ;
#10779 = VECTOR ( 'NONE', #9187, 1000.000000000000000 ) ;
#10780 = CARTESIAN_POINT ( 'NONE',  ( 25.00000000000000355, 450.0000000000000568, -105.0000000000000000 ) ) ;
#10781 = ITEM_DEFINED_TRANSFORMATION ( 'NONE', 'NONE', #9317,  #1612 ) ;
#10782 = ORIENTED_EDGE ( 'NONE', *, *, #6203, .F. ) ;
#10783 = CARTESIAN_POINT ( 'NONE',  ( -2.708734125000000326, 113.8124999986344079, 3.317242575922457132E-16 ) ) ;
#10784 = ORIENTED_EDGE ( 'NONE', *, *, #1551, .F. ) ;
#10785 = CARTESIAN_POINT ( 'NONE',  ( 28.78580657183880476, 87.64875042622801971, 9.783922737503322864 ) ) ;
#10786 = CARTESIAN_POINT ( 'NONE',  ( -11.74466661846254034, 19.32863853742761862, 74.07568943800757211 ) ) ;
#10787 = ORIENTED_EDGE ( 'NONE', *, *, #1209, .T. ) ;
#10788 = CARTESIAN_POINT ( 'NONE',  ( 0.000000000000000000, 260.0000000000000000, 0.000000000000000000 ) ) ;
#10789 = CYLINDRICAL_SURFACE ( 'NONE', #8465, 3.250000000000000444 ) ;
#10790 = VERTEX_POINT ( 'NONE', #9710 ) ;
#10791 = PLANE ( 'NONE',  #2663 ) ;
#10792 = CARTESIAN_POINT ( 'NONE',  ( 74.16198487095665826, 0.000000000000000000, -25.00000000000000000 ) ) ;
#10793 = CARTESIAN_POINT ( 'NONE',  ( -0.9407811293054709756, 43.00000000000008527, 79.50000000000000000 ) ) ;
#10794 = VERTEX_POINT ( 'NONE', #3058 ) ;
#10795 = CARTESIAN_POINT ( 'NONE',  ( 0.000000000000000000, 92.00000000000000000, 0.000000000000000000 ) ) ;
#10796 = TOROIDAL_SURFACE ( 'NONE', #9191, 17.00000000000000000, 0.5000000000000004441 ) ;
#10797 = EDGE_CURVE ( 'NONE', #7105, #6133, #623, .T. ) ;
#10798 = CARTESIAN_POINT ( 'NONE',  ( 69.55864520994451539, 18.66433107818797055, 28.04631938806005564 ) ) ;
#10799 = VERTEX_POINT ( 'NONE', #7792 ) ;
#10800 = CARTESIAN_POINT ( 'NONE',  ( 2.298097038856279806, 111.9999999972688158, 2.298097038856279806 ) ) ;
#10801 = CARTESIAN_POINT ( 'NONE',  ( 70.03799559100568217, 45.08708461952503654, -26.82731484558848578 ) ) ;
#10802 = ORIENTED_EDGE ( 'NONE', *, *, #6054, .T. ) ;
#10803 = DIRECTION ( 'NONE',  ( 0.000000000000000000, 0.000000000000000000, 1.000000000000000000 ) ) ;
#10804 = CARTESIAN_POINT ( 'NONE',  ( 71.13616097333213872, 43.15315690759868517, 23.96252879557600934 ) ) ;
#10805 = VECTOR ( 'NONE', #110, 1000.000000000000114 ) ;
#10806 = ORIENTED_EDGE ( 'NONE', *, *, #1760, .F. ) ;
#10807 = DIRECTION ( 'NONE',  ( 0.000000000000000000, 1.000000000000000000, 0.000000000000000000 ) ) ;
#10808 = CARTESIAN_POINT ( 'NONE',  ( 25.00000000000000000, 450.0000000000000568, -59.99999999999999289 ) ) ;
#10809 = SURFACE_SIDE_STYLE ('',( #8809 ) ) ;
#10810 = CARTESIAN_POINT ( 'NONE',  ( 1.734723475976807094E-14, 63.00000000000000000, 57.08203932499370836 ) ) ;
#10811 = EDGE_CURVE ( 'NONE', #12288, #7224, #5746, .T. ) ;
#10812 = EDGE_CURVE ( 'NONE', #3922, #1521, #11609, .T. ) ;
#10813 = ORIENTED_EDGE ( 'NONE', *, *, #5520, .F. ) ;
#10814 = VERTEX_POINT ( 'NONE', #8780 ) ;
#10815 = CIRCLE ( 'NONE', #10620, 5.000000000000004441 ) ;
#10816 = CARTESIAN_POINT ( 'NONE',  ( 73.35315233757310693, 19.78571428571397917, 34.26986240689829089 ) ) ;
#10817 = DIRECTION ( 'NONE',  ( 0.000000000000000000, 0.000000000000000000, 1.000000000000000000 ) ) ;
#10818 = DIRECTION ( 'NONE',  ( 0.000000000000000000, 0.000000000000000000, 1.000000000000000000 ) ) ;
#10819 = CARTESIAN_POINT ( 'NONE',  ( 30.25776724459628753, 76.75431408359612817, -5.085794527760020500 ) ) ;
#10820 = EDGE_CURVE ( 'NONE', #5250, #1500, #8380, .T. ) ;
#10821 = ADVANCED_FACE ( 'NONE', ( #6861 ), #1008, .F. ) ;
#10822 = AXIS2_PLACEMENT_3D ( 'NONE', #6456, #1593, #9059 ) ;
#10823 = VECTOR ( 'NONE', #10715, 1000.000000000000000 ) ;
#10824 = DIRECTION ( 'NONE',  ( -0.000000000000000000, -1.000000000000000000, -0.000000000000000000 ) ) ;
#10825 = CARTESIAN_POINT ( 'NONE',  ( 1.990051048614449116E-16, 110.2500000000000000, 3.250000000000000444 ) ) ;
#10826 = ORIENTED_EDGE ( 'NONE', *, *, #11085, .T. ) ;
#10827 = LINE ( 'NONE', #4402, #1605 ) ;
#10828 = VECTOR ( 'NONE', #2384, 1000.000000000000000 ) ;
#10829 = EDGE_CURVE ( 'NONE', #6133, #4828, #4114, .T. ) ;
#10830 = ORIENTED_EDGE ( 'NONE', *, *, #7376, .T. ) ;
#10831 = EDGE_CURVE ( 'NONE', #2607, #6665, #7584, .T. ) ;
#10832 = DIRECTION ( 'NONE',  ( 0.2207553928441711999, 0.8446598678744386968, -0.4876646020909775059 ) ) ;
#10833 = EDGE_LOOP ( 'NONE', ( #9163, #4476, #403 ) ) ;
#10834 = DIRECTION ( 'NONE',  ( 0.000000000000000000, 0.000000000000000000, 1.000000000000000000 ) ) ;
#10835 = FACE_OUTER_BOUND ( 'NONE', #9319, .T. ) ;
#10836 = VERTEX_POINT ( 'NONE', #9591 ) ;
#10837 = CARTESIAN_POINT ( 'NONE',  ( 27.31079997599232456, 86.91362087007181003, 12.41453806599178478 ) ) ;
#10838 = FACE_OUTER_BOUND ( 'NONE', #8277, .T. ) ;
#10839 = TOROIDAL_SURFACE ( 'NONE', #7855, 90.00000000000002842, 10.00000000000000000 ) ;
#10840 = ORIENTED_EDGE ( 'NONE', *, *, #368, .T. ) ;
#10841 = CARTESIAN_POINT ( 'NONE',  ( 70.01409082250448535, 44.97240956491599917, -26.88960057466319498 ) ) ;
#10842 = CIRCLE ( 'NONE', #4883, 125.0000000000000568 ) ;
#10843 = ORIENTED_EDGE ( 'NONE', *, *, #7016, .F. ) ;
#10844 = ADVANCED_FACE ( 'NONE', ( #2125, #11545 ), #5057, .F. ) ;
#10845 = CARTESIAN_POINT ( 'NONE',  ( 107.1104145097471445, 285.0000000000000568, 41.86118851096031079 ) ) ;
#10846 = DIRECTION ( 'NONE',  ( 0.000000000000000000, 1.000000000000000000, 0.000000000000000000 ) ) ;
#10847 = AXIS2_PLACEMENT_3D ( 'NONE', #7808, #3133, #10674 ) ;
#10848 = VERTEX_POINT ( 'NONE', #7904 ) ;
#10849 = AXIS2_PLACEMENT_3D ( 'NONE', #2251, #6181, #6122 ) ;
#10850 = DIRECTION ( 'NONE',  ( 0.000000000000000000, -0.000000000000000000, 1.000000000000000000 ) ) ;
#10851 = DIRECTION ( 'NONE',  ( -0.000000000000000000, 1.000000000000000000, -0.000000000000000000 ) ) ;
#10852 = ORIENTED_EDGE ( 'NONE', *, *, #8771, .F. ) ;
#10853 = CARTESIAN_POINT ( 'NONE',  ( 0.000000000000000000, 265.0000000000000000, 0.000000000000000000 ) ) ;
#10854 = CARTESIAN_POINT ( 'NONE',  ( 10.19254911989241386, 23.71650635094626836, 80.00000000000000000 ) ) ;
#10855 = DIRECTION ( 'NONE',  ( 0.000000000000000000, 0.000000000000000000, 1.000000000000000000 ) ) ;
#10856 = ORIENTED_EDGE ( 'NONE', *, *, #8392, .T. ) ;
#10857 = CARTESIAN_POINT ( 'NONE',  ( 2.708734124999999882, 110.5624999986344079, 0.000000000000000000 ) ) ;
#10858 = CARTESIAN_POINT ( 'NONE',  ( 71.69656859387025349, 15.34954140224283847, 22.14271594285881051 ) ) ;
#10859 = VECTOR ( 'NONE', #2947, 1000.000000000000000 ) ;
#10860 = AXIS2_PLACEMENT_3D ( 'NONE', #11539, #5862, #3053 ) ;
#10861 = EDGE_LOOP ( 'NONE', ( #5892, #11801 ) ) ;
#10862 = DIRECTION ( 'NONE',  ( 0.000000000000000000, 1.000000000000000000, 0.000000000000000000 ) ) ;
#10863 = DIRECTION ( 'NONE',  ( 0.000000000000000000, 1.000000000000000000, 0.000000000000000000 ) ) ;
#10864 = ORIENTED_EDGE ( 'NONE', *, *, #7228, .F. ) ;
#10865 = CARTESIAN_POINT ( 'NONE',  ( 0.000000000000000000, 290.0000000000000568, -110.0000000000000284 ) ) ;
#10866 = CARTESIAN_POINT ( 'NONE',  ( 71.05921646411503900, 42.81507391128047857, 24.19824146092189920 ) ) ;
#10867 = EDGE_LOOP ( 'NONE', ( #11779, #6145, #10371, #2547 ) ) ;
#10868 = EDGE_CURVE ( 'NONE', #11220, #4828, #11782, .T. ) ;
#10869 = PLANE ( 'NONE',  #5034 ) ;
#10870 = AXIS2_PLACEMENT_3D ( 'NONE', #4492, #8344, #2679 ) ;
#10871 = CARTESIAN_POINT ( 'NONE',  ( 140.0000000000011369, 230.0000000000000853, 20.00000000000000000 ) ) ;
#10872 = CIRCLE ( 'NONE', #10268, 5.000000000000004441 ) ;
#10873 = ADVANCED_FACE ( 'NONE', ( #7847 ), #2024, .T. ) ;
#10874 = CARTESIAN_POINT ( 'NONE',  ( 0.000000000000000000, 87.00000000000000000, 0.000000000000000000 ) ) ;
#10875 = CARTESIAN_POINT ( 'NONE',  ( -2.708734125000000326, 113.7499999986344221, 1.121994411437819084 ) ) ;
#10876 =( GEOMETRIC_REPRESENTATION_CONTEXT ( 3 ) GLOBAL_UNCERTAINTY_ASSIGNED_CONTEXT ( ( #8124 ) ) GLOBAL_UNIT_ASSIGNED_CONTEXT ( ( #7701, #4769, #5027 ) ) REPRESENTATION_CONTEXT ( 'NONE', 'WORKASPACE' ) );
#10877 = VERTEX_POINT ( 'NONE', #2177 ) ;
#10878 = SURFACE_SIDE_STYLE ('',( #7937 ) ) ;
#10879 = VERTEX_POINT ( 'NONE', #5807 ) ;
#10880 = CIRCLE ( 'NONE', #8689, 15.00000000000000000 ) ;
#10881 = CARTESIAN_POINT ( 'NONE',  ( 10.15088245323607907, 36.35566243268468867, 80.00000048127353125 ) ) ;
#10882 = EDGE_CURVE ( 'NONE', #11846, #2311, #4870, .T. ) ;
#10883 = DIRECTION ( 'NONE',  ( 1.000000000000000000, -0.000000000000000000, 1.224646799147353207E-16 ) ) ;
#10884 = CARTESIAN_POINT ( 'NONE',  ( 0.000000000000000000, 92.00000000000000000, 0.000000000000000000 ) ) ;
#10885 = DIRECTION ( 'NONE',  ( 0.000000000000000000, -0.000000000000000000, 1.000000000000000000 ) ) ;
#10886 = DIRECTION ( 'NONE',  ( -0.000000000000000000, -1.000000000000000000, -0.000000000000000000 ) ) ;
#10887 = SHAPE_DEFINITION_REPRESENTATION ( #2790, #11842 ) ;
#10888 = LINE ( 'NONE', #11708, #11843 ) ;
#10889 = CARTESIAN_POINT ( 'NONE',  ( 1.121994411437819528, 112.1249999986343937, -2.708734124999999882 ) ) ;
#10890 = EDGE_LOOP ( 'NONE', ( #3292, #11725, #6926, #11454 ) ) ;
#10891 = LINE ( 'NONE', #10013, #1213 ) ;
#10892 = ADVANCED_FACE ( 'NONE', ( #10597 ), #5177, .T. ) ;
#10893 = EDGE_CURVE ( 'NONE', #5925, #10404, #11911, .T. ) ;
#10894 = ORIENTED_EDGE ( 'NONE', *, *, #6485, .T. ) ;
#10895 = LINE ( 'NONE', #6159, #5242 ) ;
#10896 = VERTEX_POINT ( 'NONE', #2359 ) ;
#10897 = FACE_BOUND ( 'NONE', #5157, .T. ) ;
#10898 = CARTESIAN_POINT ( 'NONE',  ( 75.04216158314673635, 16.80959580454246094, -23.86402193374160774 ) ) ;
#10899 = VERTEX_POINT ( 'NONE', #5238 ) ;
#10900 = CARTESIAN_POINT ( 'NONE',  ( -12.32411137850303184, 36.71650635094619730, 79.50000000000000000 ) ) ;
#10901 = CARTESIAN_POINT ( 'NONE',  ( -29.92433840049366012, 87.25972750007186107, -9.110115264091719567 ) ) ;
#10902 = ORIENTED_EDGE ( 'NONE', *, *, #338, .F. ) ;
#10903 = CARTESIAN_POINT ( 'NONE',  ( 71.40042903152233578, 48.95734231283034177, -22.96380533506442845 ) ) ;
#10904 = AXIS2_PLACEMENT_3D ( 'NONE', #1563, #10148, #4356 ) ;
#10905 = ORIENTED_EDGE ( 'NONE', *, *, #7891, .F. ) ;
#10906 = CARTESIAN_POINT ( 'NONE',  ( 30.56632211525506548, 87.12700276260753185, 8.880229275382253817 ) ) ;
#10907 = CARTESIAN_POINT ( 'NONE',  ( 0.000000000000000000, 165.5000000000000000, 0.000000000000000000 ) ) ;
#10908 = ORIENTED_EDGE ( 'NONE', *, *, #5977, .F. ) ;
#10909 = DIRECTION ( 'NONE',  ( 0.4999999999999878431, -0.8660254037844455910, 0.000000000000000000 ) ) ;
#10910 = CARTESIAN_POINT ( 'NONE',  ( 0.000000000000000000, 10.00000000000017586, 0.000000000000000000 ) ) ;
#10911 = VECTOR ( 'NONE', #5401, 1000.000000000000000 ) ;
#10912 = ORIENTED_EDGE ( 'NONE', *, *, #9960, .F. ) ;
#10913 = STYLED_ITEM ( 'NONE', ( #2023 ), #11672 ) ;
#10914 = DIRECTION ( 'NONE',  ( -0.000000000000000000, -1.000000000000000000, -0.000000000000000000 ) ) ;
#10915 = DIRECTION ( 'NONE',  ( 0.9595199576812789566, 0.000000000000000000, 0.2816406412635022449 ) ) ;
#10916 = CARTESIAN_POINT ( 'NONE',  ( 7.594472908539098732, 25.21650635094628257, 80.00000000000000000 ) ) ;
#10917 = ORIENTED_EDGE ( 'NONE', *, *, #11817, .T. ) ;
#10918 = CARTESIAN_POINT ( 'NONE',  ( -30.00100000000000122, 75.26794919243111792, -7.660254037844449471 ) ) ;
#10919 = ADVANCED_FACE ( 'NONE', ( #9016 ), #6978, .F. ) ;
#10920 = CARTESIAN_POINT ( 'NONE',  ( 71.89703483712752075, 15.05775874217476940, 21.44956398269973619 ) ) ;
#10921 = EDGE_CURVE ( 'NONE', #5307, #4364, #11260, .T. ) ;
#10922 = ORIENTED_EDGE ( 'NONE', *, *, #997, .T. ) ;
#10923 = CARTESIAN_POINT ( 'NONE',  ( 76.75412411316109740, 44.83621509884553546, -21.27950340534319906 ) ) ;
#10924 = DIRECTION ( 'NONE',  ( -1.387778780781445676E-14, -1.000000000000000000, 0.000000000000000000 ) ) ;
#10925 = ORIENTED_EDGE ( 'NONE', *, *, #7034, .T. ) ;
#10926 = DIRECTION ( 'NONE',  ( -0.7071067811865454633, 0.7071067811865495711, 0.000000000000000000 ) ) ;
#10927 = CARTESIAN_POINT ( 'NONE',  ( 74.30294665491157957, 41.32313156420044464, 24.82467190422428516 ) ) ;
#10928 = EDGE_LOOP ( 'NONE', ( #10141, #6739, #8949, #11747 ) ) ;
#10929 = DIRECTION ( 'NONE',  ( -0.5000000000000095479, -0.8660254037844331565, 0.000000000000000000 ) ) ;
#10930 = FACE_BOUND ( 'NONE', #173, .T. ) ;
#10931 = CARTESIAN_POINT ( 'NONE',  ( -1.121994411437820194, 113.9999999986344079, -2.708734124999999882 ) ) ;
#10932 = CIRCLE ( 'NONE', #9954, 70.00000000000001421 ) ;
#10933 =( BOUNDED_CURVE ( )  B_SPLINE_CURVE ( 2, ( #7215, #1545, #5290, #5708, #9067, #541, #3642, #3699, #2479, #4339, #11014, #1771, #11317, #8136, #4573, #7449, #2704, #2198, #9729, #7628, #14, #7868, #8552, #2956, #10616, #10553, #3018, #3829, #5946, #1210, #10736, #2143, #5016, #8798, #138, #4826, #11438, #6755, #3954, #6820, #11563, #6009, #265, #4077, #9671, #4952, #11506, #4013, #5890, #11629, #2021, #8737, #7814, #8616, #3078, #4759, #965, #2889, #11686, #3138, #6698, #5827, #6881, #2081, #10495 ),
 .UNSPECIFIED., .F., .F. ) 
 B_SPLINE_CURVE_WITH_KNOTS ( ( 3, 2, 2, 2, 2, 2, 2, 2, 2, 2, 2, 2, 2, 2, 2, 2, 2, 2, 2, 2, 2, 2, 2, 2, 2, 2, 2, 2, 2, 2, 2, 2, 3 ),
 ( 0.000000000000000000, 0.03125000000000000000, 0.06250000000000000000, 0.09375000000000000000, 0.1250000000000000000, 0.1562500000000000000, 0.1875000000000000000, 0.2187500000000000000, 0.2500000000000000000, 0.2812500000000000000, 0.3125000000000000000, 0.3437500000000000000, 0.3750000000000000000, 0.4062500000000000000, 0.4375000000000000000, 0.4687500000000000000, 0.5000000000000000000, 0.5312500000000000000, 0.5625000000000000000, 0.5937500000000000000, 0.6250000000000000000, 0.6562500000000000000, 0.6875000000000000000, 0.7187500000000000000, 0.7500000000000000000, 0.7812500000000000000, 0.8125000000000000000, 0.8437500000000000000, 0.8750000000000000000, 0.9062500000000000000, 0.9375000000000000000, 0.9687500000000000000, 1.000000000000000000 ),
 .UNSPECIFIED. ) 
 CURVE ( )  GEOMETRIC_REPRESENTATION_ITEM ( )  RATIONAL_B_SPLINE_CURVE ( ( 1.000000000000000000, 0.9238795325112867385, 1.000000000000000000, 0.9238795325112867385, 1.000000000000000000, 0.9238795325112867385, 1.000000000000000000, 0.9238795325112867385, 1.000000000000000000, 0.9238795325112867385, 1.000000000000000000, 0.9238795325112867385, 1.000000000000000000, 0.9238795325112867385, 1.000000000000000000, 0.9238795325112867385, 1.000000000000000000, 0.9238795325112867385, 1.000000000000000000, 0.9238795325112867385, 1.000000000000000000, 0.9238795325112867385, 1.000000000000000000, 0.9238795325112867385, 1.000000000000000000, 0.9238795325112867385, 1.000000000000000000, 0.9238795325112867385, 1.000000000000000000, 0.9238795325112867385, 1.000000000000000000, 0.9238795325112867385, 1.000000000000000000, 0.9238795325112867385, 1.000000000000000000, 0.9238795325112867385, 1.000000000000000000, 0.9238795325112867385, 1.000000000000000000, 0.9238795325112867385, 1.000000000000000000, 0.9238795325112867385, 1.000000000000000000, 0.9238795325112867385, 1.000000000000000000, 0.9238795325112867385, 1.000000000000000000, 0.9238795325112867385, 1.000000000000000000, 0.9238795325112867385, 1.000000000000000000, 0.9238795325112867385, 1.000000000000000000, 0.9238795325112867385, 1.000000000000000000, 0.9238795325112867385, 1.000000000000000000, 0.9238795325112867385, 1.000000000000000000, 0.9238795325112867385, 1.000000000000000000, 0.9238795325112867385, 1.000000000000000000, 0.9238795325112867385, 1.000000000000000000 ) ) 
 REPRESENTATION_ITEM ( '' )  );
#10934 = EDGE_LOOP ( 'NONE', ( #10429, #8776 ) ) ;
#10935 = ORIENTED_EDGE ( 'NONE', *, *, #3046, .F. ) ;
#10936 =( LENGTH_UNIT ( ) NAMED_UNIT ( * ) SI_UNIT ( .MILLI., .METRE. ) );
#10937 = ORIENTED_EDGE ( 'NONE', *, *, #9205, .T. ) ;
#10938 = AXIS2_PLACEMENT_3D ( 'NONE', #5670, #10140, #1618 ) ;
#10939 = CARTESIAN_POINT ( 'NONE',  ( 8.572527594031474570E-15, -5.000000000000000000, -70.00000000000001421 ) ) ;
#10940 = FACE_OUTER_BOUND ( 'NONE', #5428, .T. ) ;
#10941 = CARTESIAN_POINT ( 'NONE',  ( 3.061616997868382648E-15, 87.00000000000000000, -24.99999999999999645 ) ) ;
#10942 = CYLINDRICAL_SURFACE ( 'NONE', #4608, 3.250000000000000444 ) ;
#10943 = DIRECTION ( 'NONE',  ( 0.000000000000000000, 0.000000000000000000, -1.000000000000000000 ) ) ;
#10944 = CARTESIAN_POINT ( 'NONE',  ( 32.78711330112231792, 75.47285661897714704, -7.305343964218459440 ) ) ;
#10945 = FACE_OUTER_BOUND ( 'NONE', #5770, .T. ) ;
#10946 = PLANE ( 'NONE',  #7256 ) ;
#10947 = CARTESIAN_POINT ( 'NONE',  ( -2.708734125000000770, 110.8749999986343937, -1.121994411437818639 ) ) ;
#10948 = AXIS2_PLACEMENT_3D ( 'NONE', #6600, #935, #12160 ) ;
#10949 = PLANE ( 'NONE',  #2405 ) ;
#10950 = DIRECTION ( 'NONE',  ( -1.000000000000000000, 0.000000000000000000, 0.000000000000000000 ) ) ;
#10951 = EDGE_CURVE ( 'NONE', #3270, #1577, #5300, .T. ) ;
#10952 = SHAPE_REPRESENTATION ( 'Locking Bowl Cover with Feed Chute', ( #1612 ), #3176 ) ;
#10953 = VERTEX_POINT ( 'NONE', #11852 ) ;
#10954 = VECTOR ( 'NONE', #1546, 1000.000000000000000 ) ;
#10955 = CARTESIAN_POINT ( 'NONE',  ( 10.19254911989241386, 23.71650635094626836, 80.00000000000000000 ) ) ;
#10956 = ORIENTED_EDGE ( 'NONE', *, *, #10494, .T. ) ;
#10957 = AXIS2_PLACEMENT_3D ( 'NONE', #10808, #11882, #6200 ) ;
#10958 = CARTESIAN_POINT ( 'NONE',  ( 0.000000000000000000, 52.00000000000000711, 0.000000000000000000 ) ) ;
#10959 = CYLINDRICAL_SURFACE ( 'NONE', #6898, 9.999999999999994671 ) ;
#10960 = ORIENTED_EDGE ( 'NONE', *, *, #7521, .T. ) ;
#10961 = LINE ( 'NONE', #2423, #5856 ) ;
#10962 = CARTESIAN_POINT ( 'NONE',  ( -0.9407811293054709756, 43.00000000000008527, 80.00000000000000000 ) ) ;
#10963 = EDGE_CURVE ( 'NONE', #10848, #5904, #4232, .T. ) ;
#10964 = EDGE_CURVE ( 'NONE', #8921, #12045, #9972, .T. ) ;
#10965 = VERTEX_POINT ( 'NONE', #11027 ) ;
#10966 = CARTESIAN_POINT ( 'NONE',  ( 69.57537924859245493, 41.62899728819233758, -28.00483409347995689 ) ) ;
#10967 = VECTOR ( 'NONE', #10239, 1000.000000000000114 ) ;
#10968 = ORIENTED_EDGE ( 'NONE', *, *, #8805, .F. ) ;
#10969 = CIRCLE ( 'NONE', #7593, 115.0000000000000284 ) ;
#10970 = LINE ( 'NONE', #6116, #9303 ) ;
#10971 = DIRECTION ( 'NONE',  ( -0.4999999999999978351, 0.000000000000000000, 0.8660254037844399289 ) ) ;
#10972 = EDGE_LOOP ( 'NONE', ( #5031, #7221 ) ) ;
#10973 = EDGE_LOOP ( 'NONE', ( #5055, #5697, #7860, #9716 ) ) ;
#10974 = CARTESIAN_POINT ( 'NONE',  ( 0.000000000000000000, 122.0000000000000000, 0.000000000000000000 ) ) ;
#10975 = EDGE_CURVE ( 'NONE', #2554, #12106, #10081, .T. ) ;
#10976 = DIRECTION ( 'NONE',  ( -1.000000000000000000, -0.000000000000000000, -0.000000000000000000 ) ) ;
#10977 = VECTOR ( 'NONE', #11235, 1000.000000000000000 ) ;
#10978 = ORIENTED_EDGE ( 'NONE', *, *, #8899, .F. ) ;
#10979 = DIRECTION ( 'NONE',  ( 1.000000000000000000, 0.000000000000000000, 0.000000000000000000 ) ) ;
#10980 = DIRECTION ( 'NONE',  ( 0.000000000000000000, 1.000000000000000000, 0.000000000000000000 ) ) ;
#10981 = PLANE ( 'NONE',  #6991 ) ;
#10982 = ORIENTED_EDGE ( 'NONE', *, *, #3540, .T. ) ;
#10983 = CARTESIAN_POINT ( 'NONE',  ( 1.658621287961228320E-16, 110.8124999986344079, 2.708734124999999882 ) ) ;
#10984 = CIRCLE ( 'NONE', #7201, 10.00000000000000178 ) ;
#10985 = CARTESIAN_POINT ( 'NONE',  ( 71.00573438501008638, 11.81969099518210520, 24.15070487907408037 ) ) ;
#10986 = CIRCLE ( 'NONE', #2221, 9.999999999999998224 ) ;
#10987 = ORIENTED_EDGE ( 'NONE', *, *, #11628, .T. ) ;
#10988 = CARTESIAN_POINT ( 'NONE',  ( 77.12362621866023460, 15.03061249690207291, 20.63427607811778230 ) ) ;
#10989 = CARTESIAN_POINT ( 'NONE',  ( 0.000000000000000000, 110.0000000000000000, 0.000000000000000000 ) ) ;
#10990 = ORIENTED_EDGE ( 'NONE', *, *, #214, .T. ) ;
#10991 = EDGE_CURVE ( 'NONE', #298, #2246, #1388, .T. ) ;
#10992 = DIRECTION ( 'NONE',  ( 0.000000000000000000, 0.000000000000000000, 1.000000000000000000 ) ) ;
#10993 = EDGE_CURVE ( 'NONE', #6913, #9588, #5360, .T. ) ;
#10994 = CARTESIAN_POINT ( 'NONE',  ( 75.64998878962165918, 43.99497189443935952, 23.01105902605777231 ) ) ;
#10995 = EDGE_LOOP ( 'NONE', ( #3489, #3400 ) ) ;
#10996 = SPHERICAL_SURFACE ( 'NONE', #5502, 5.000000000000000000 ) ;
#10997 = PLANE ( 'NONE',  #4113 ) ;
#10998 = CARTESIAN_POINT ( 'NONE',  ( 1.915364268218909594, 111.4374999986344079, 1.915364268218909594 ) ) ;
#10999 = CIRCLE ( 'NONE', #5630, 70.00000000000001421 ) ;
#11000 = ORIENTED_EDGE ( 'NONE', *, *, #6395, .F. ) ;
#11001 = EDGE_LOOP ( 'NONE', ( #1075, #2439, #10526 ) ) ;
#11002 = CIRCLE ( 'NONE', #6035, 10.49999999999999822 ) ;
#11003 = UNCERTAINTY_MEASURE_WITH_UNIT (LENGTH_MEASURE( 1.000000000000000082E-05 ), #7995, 'distance_accuracy_value', 'NONE');
#11004 = LINE ( 'NONE', #12077, #11431 ) ;
#11005 = CARTESIAN_POINT ( 'NONE',  ( 165.0000000000011369, 225.0000000000000853, -19.99999999999999645 ) ) ;
#11006 = DIRECTION ( 'NONE',  ( 1.000000000000000000, 0.000000000000000000, 0.000000000000000000 ) ) ;
#11007 = CARTESIAN_POINT ( 'NONE',  ( 1.990051048614449116E-16, 112.2500000000000000, 3.250000000000000444 ) ) ;
#11008 = DIRECTION ( 'NONE',  ( 0.000000000000000000, -1.000000000000000000, 1.287488025362403787E-15 ) ) ;
#11009 = CARTESIAN_POINT ( 'NONE',  ( 121.4644660940682428, 46.46446609406732620, 20.00000000000000000 ) ) ;
#11010 = DIRECTION ( 'NONE',  ( 0.000000000000000000, 0.000000000000000000, 1.000000000000000000 ) ) ;
#11011 = DIRECTION ( 'NONE',  ( 0.000000000000000000, 0.000000000000000000, 1.000000000000000000 ) ) ;
#11012 = CARTESIAN_POINT ( 'NONE',  ( -1.121994411437818862, 111.6249999986344079, 2.708734125000000326 ) ) ;
#11013 = AXIS2_PLACEMENT_3D ( 'NONE', #4656, #12274, #7527 ) ;
#11014 = CARTESIAN_POINT ( 'NONE',  ( -1.915364268218909594, 111.1874999986344079, -1.915364268218908927 ) ) ;
#11015 = DIRECTION ( 'NONE',  ( 1.224646799147353207E-16, 1.000000000000000000, -0.000000000000000000 ) ) ;
#11016 = B_SPLINE_CURVE_WITH_KNOTS ( 'NONE', 3,
 ( #3884, #5818, #7621, #7806, #5938, #6933, #2882, #11429, #9603, #6690, #1017, #4818, #8606, #5132, #11803, #11986, #3443, #2191, #7913, #3246, #7239, #9089, #5999, #6059 ),
 .UNSPECIFIED., .F., .F.,
 ( 4, 2, 2, 2, 2, 2, 2, 2, 2, 2, 2, 4 ),
 ( 0.000000000000000000, 0.0009796746052621193267, 0.001959349210524238653, 0.003918698421048477307, 0.004898373026310590128, 0.005878047631572703817, 0.007837396842096925123, 0.009796746052621145562, 0.01175609526314536774, 0.01273576986840747882, 0.01371544447366958817, 0.01567479368419381902 ),
 .UNSPECIFIED. ) ;
#11017 = ORIENTED_EDGE ( 'NONE', *, *, #2280, .T. ) ;
#11018 = CIRCLE ( 'NONE', #5657, 0.5000000000000004441 ) ;
#11019 = CARTESIAN_POINT ( 'NONE',  ( 0.000000000000000000, 265.0000000000000000, 0.000000000000000000 ) ) ;
#11020 = ORIENTED_EDGE ( 'NONE', *, *, #11812, .F. ) ;
#11021 = CARTESIAN_POINT ( 'NONE',  ( 1.200153863164406345E-14, 265.0000000000000000, 98.00000000000001421 ) ) ;
#11022 = CARTESIAN_POINT ( 'NONE',  ( 76.77294714683046095, 15.14884821498869094, -21.25082451143516948 ) ) ;
#11023 = ORIENTED_EDGE ( 'NONE', *, *, #5030, .T. ) ;
#11024 = EDGE_CURVE ( 'NONE', #4325, #4065, #5366, .T. ) ;
#11025 = CARTESIAN_POINT ( 'NONE',  ( 25.00000000000000000, 445.0000000000000568, -59.99999999999999289 ) ) ;
#11026 = ADVANCED_FACE ( 'NONE', ( #7104 ), #4350, .T. ) ;
#11027 = CARTESIAN_POINT ( 'NONE',  ( 117.9289321881355193, 45.00000000000008527, -20.00000000000000000 ) ) ;
#11028 = ORIENTED_EDGE ( 'NONE', *, *, #10797, .F. ) ;
#11029 = CARTESIAN_POINT ( 'NONE',  ( 145.0000000000011369, 67.07106781186550393, 25.00000000000000000 ) ) ;
#11030 =( GEOMETRIC_REPRESENTATION_CONTEXT ( 3 ) GLOBAL_UNCERTAINTY_ASSIGNED_CONTEXT ( ( #3405 ) ) GLOBAL_UNIT_ASSIGNED_CONTEXT ( ( #8494, #2765, #12316 ) ) REPRESENTATION_CONTEXT ( 'NONE', 'WORKASPACE' ) );
#11031 =( BOUNDED_SURFACE ( )  B_SPLINE_SURFACE ( 3, 2, ( 
 ( #11981, #1685, #3553 ),
 ( #4423, #626, #12104 ),
 ( #7234, #1745, #688 ),
 ( #5365, #5430, #4545 ) ),
 .UNSPECIFIED., .F., .F., .F. ) 
 B_SPLINE_SURFACE_WITH_KNOTS ( ( 4, 4 ),
 ( 3, 3 ),
 ( 1.665911834627059607, 1.695449464845517618 ),
 ( 0.2468956587999593388, 1.000000000000000000 ),
 .UNSPECIFIED. ) 
 GEOMETRIC_REPRESENTATION_ITEM ( )  RATIONAL_B_SPLINE_SURFACE ( (
 ( 0.8800340755151767613, 0.7570513692546891882, 1.000000000000000000),
 ( 0.8788691223080344894, 0.7546921677749939272, 1.000000000000000000),
 ( 0.8776977286441711712, 0.7523199234237630817, 1.000000000000000000),
 ( 0.8765201392483088494, 0.7499351318045301973, 1.000000000000000000) ) ) 
 REPRESENTATION_ITEM ( '' )  SURFACE ( )  );
#11032 = VECTOR ( 'NONE', #6293, 1000.000000000000000 ) ;
#11033 = ORIENTED_EDGE ( 'NONE', *, *, #7673, .F. ) ;
#11034 = CARTESIAN_POINT ( 'NONE',  ( -1.440781129305282571, 17.00000000000009592, 79.50000000000000000 ) ) ;
#11035 = CARTESIAN_POINT ( 'NONE',  ( 0.000000000000000000, 340.0000000000000000, -110.0000000000000284 ) ) ;
#11036 = ORIENTED_EDGE ( 'NONE', *, *, #1177, .F. ) ;
#11037 = VERTEX_POINT ( 'NONE', #6112 ) ;
#11038 = FACE_OUTER_BOUND ( 'NONE', #3990, .T. ) ;
#11039 = DIRECTION ( 'NONE',  ( 6.938893903907228378E-17, 0.000000000000000000, -1.000000000000000000 ) ) ;
#11040 = ORIENTED_EDGE ( 'NONE', *, *, #4104, .T. ) ;
#11041 = EDGE_CURVE ( 'NONE', #11684, #2560, #12339, .T. ) ;
#11042 = FACE_OUTER_BOUND ( 'NONE', #1816, .T. ) ;
#11043 = AXIS2_PLACEMENT_3D ( 'NONE', #10989, #10046, #1520 ) ;
#11044 = FACE_OUTER_BOUND ( 'NONE', #1088, .T. ) ;
#11045 = FACE_OUTER_BOUND ( 'NONE', #6511, .T. ) ;
#11046 = ORIENTED_EDGE ( 'NONE', *, *, #12117, .F. ) ;
#11047 = CARTESIAN_POINT ( 'NONE',  ( 0.000000000000000000, 127.0000000000000000, 0.000000000000000000 ) ) ;
#11048 = ADVANCED_FACE ( 'NONE', ( #10838 ), #587, .T. ) ;
#11049 = CARTESIAN_POINT ( 'NONE',  ( 71.13813068160065711, 16.85611227734841933, 23.95492789737738804 ) ) ;
#11050 = AXIS2_PLACEMENT_3D ( 'NONE', #1245, #1306, #3296 ) ;
#11051 = AXIS2_PLACEMENT_3D ( 'NONE', #8778, #2995, #6799 ) ;
#11052 = ORIENTED_EDGE ( 'NONE', *, *, #4179, .F. ) ;
#11053 = EDGE_CURVE ( 'NONE', #4065, #4325, #10130, .T. ) ;
#11054 = CARTESIAN_POINT ( 'NONE',  ( 30.00100000000000122, 85.26794919243110371, -9.660254037844429931 ) ) ;
#11055 = EDGE_CURVE ( 'NONE', #4148, #938, #1786, .T. ) ;
#11056 = DIRECTION ( 'NONE',  ( 0.000000000000000000, 0.000000000000000000, 1.000000000000000000 ) ) ;
#11057 = ORIENTED_EDGE ( 'NONE', *, *, #10206, .F. ) ;
#11058 = FACE_OUTER_BOUND ( 'NONE', #3583, .T. ) ;
#11059 = CARTESIAN_POINT ( 'NONE',  ( 75.74050859682202486, 44.09128781609246772, 22.87883167916283256 ) ) ;
#11060 = ORIENTED_EDGE ( 'NONE', *, *, #2955, .F. ) ;
#11061 = DIRECTION ( 'NONE',  ( 1.000000000000000000, 0.000000000000000000, 0.000000000000000000 ) ) ;
#11062 = CARTESIAN_POINT ( 'NONE',  ( 25.00000000000000355, 347.0000000000000568, -88.00000000000000000 ) ) ;
#11063 = CARTESIAN_POINT ( 'NONE',  ( -2.708734125000000326, 111.8124999986344079, 3.317242575922457132E-16 ) ) ;
#11064 = VECTOR ( 'NONE', #6814, 1000.000000000000000 ) ;
#11065 = CARTESIAN_POINT ( 'NONE',  ( -4.975863863883684959E-16, 112.3124999986344079, -2.708734124999999882 ) ) ;
#11066 = ORIENTED_EDGE ( 'NONE', *, *, #8599, .F. ) ;
#11067 = EDGE_LOOP ( 'NONE', ( #8026, #6719, #9987, #11652 ) ) ;
#11068 = AXIS2_PLACEMENT_3D ( 'NONE', #7567, #5582, #11375 ) ;
#11069 = SURFACE_STYLE_FILL_AREA ( #6452 ) ;
#11070 = CONICAL_SURFACE ( 'NONE', #309, 75.00000000000001421, 0.7853981633974427279 ) ;
#11071 = AXIS2_PLACEMENT_3D ( 'NONE', #6874, #5700, #7859 ) ;
#11072 = CARTESIAN_POINT ( 'NONE',  ( 9.942549119892413856, 23.28349364905404428, 79.50000000000000000 ) ) ;
#11073 = CARTESIAN_POINT ( 'NONE',  ( 24.76446302067271077, 285.0000000000000568, -102.0378428393002963 ) ) ;
#11074 = LINE ( 'NONE', #2769, #4624 ) ;
#11075 = PLANE ( 'NONE',  #2029 ) ;
#11076 = VECTOR ( 'NONE', #8714, 1000.000000000000114 ) ;
#11077 = CARTESIAN_POINT ( 'NONE',  ( 9.942549119892305498, 36.71650635094628967, 79.50000000000000000 ) ) ;
#11078 = CARTESIAN_POINT ( 'NONE',  ( -16.08467657231584624, 32.05922307041088004, 73.25523918613529872 ) ) ;
#11079 = CARTESIAN_POINT ( 'NONE',  ( 74.16198487095664404, 20.00000000000009237, -29.99999999999999645 ) ) ;
#11080 = LINE ( 'NONE', #7278, #3474 ) ;
#11081 = CYLINDRICAL_SURFACE ( 'NONE', #7358, 9.999999999999998224 ) ;
#11082 = LINE ( 'NONE', #8322, #8947 ) ;
#11083 = EDGE_CURVE ( 'NONE', #6351, #11360, #9267, .T. ) ;
#11084 = VECTOR ( 'NONE', #11824, 1000.000000000000114 ) ;
#11085 = EDGE_CURVE ( 'NONE', #1902, #7629, #680, .T. ) ;
#11086 = CARTESIAN_POINT ( 'NONE',  ( 1.857738790484679381, 15.28369354803722402, 74.98235353336227149 ) ) ;
#11087 = ORIENTED_EDGE ( 'NONE', *, *, #671, .T. ) ;
#11088 = LINE ( 'NONE', #8328, #8812 ) ;
#11089 = VERTEX_POINT ( 'NONE', #871 ) ;
#11090 = LINE ( 'NONE', #11021, #7272 ) ;
#11091 = CARTESIAN_POINT ( 'NONE',  ( 3.249999999999999556, 113.8124999972688016, -1.346194077712561166 ) ) ;
#11092 = ORIENTED_EDGE ( 'NONE', *, *, #8754, .F. ) ;
#11093 = CARTESIAN_POINT ( 'NONE',  ( -1.440781129305471087, 43.00000000000008527, 80.00000000000000000 ) ) ;
#11094 = AXIS2_PLACEMENT_3D ( 'NONE', #9806, #1283, #5090 ) ;
#11095 = FACE_OUTER_BOUND ( 'NONE', #716, .T. ) ;
#11096 = VERTEX_POINT ( 'NONE', #1796 ) ;
#11097 = DIRECTION ( 'NONE',  ( 0.000000000000000000, 1.000000000000000000, 0.000000000000000000 ) ) ;
#11098 = EDGE_CURVE ( 'NONE', #1995, #3270, #3579, .T. ) ;
#11099 = EDGE_LOOP ( 'NONE', ( #993, #8648, #4051, #12255 ) ) ;
#11100 = DIRECTION ( 'NONE',  ( 0.000000000000000000, 1.000000000000000000, 0.000000000000000000 ) ) ;
#11101 = PLANE ( 'NONE',  #2052 ) ;
#11102 = ORIENTED_EDGE ( 'NONE', *, *, #7229, .F. ) ;
#11103 = CARTESIAN_POINT ( 'NONE',  ( -89.80805993797480369, 275.0000000000000000, 71.82974571984181011 ) ) ;
#11104 = DIRECTION ( 'NONE',  ( 0.000000000000000000, 0.000000000000000000, -1.000000000000000000 ) ) ;
#11105 = ORIENTED_EDGE ( 'NONE', *, *, #11354, .F. ) ;
#11106 = CARTESIAN_POINT ( 'NONE',  ( 0.000000000000000000, 275.0000000000000000, 0.000000000000000000 ) ) ;
#11107 = PLANE ( 'NONE',  #8295 ) ;
#11108 = CARTESIAN_POINT ( 'NONE',  ( 5.000000000000000888, 0.000000000000000000, 0.000000000000000000 ) ) ;
#11109 = EDGE_CURVE ( 'NONE', #6665, #2607, #7161, .T. ) ;
#11110 = VERTEX_POINT ( 'NONE', #12158 ) ;
#11111 = DIRECTION ( 'NONE',  ( 0.000000000000000000, 0.000000000000000000, -1.000000000000000000 ) ) ;
#11112 = CARTESIAN_POINT ( 'NONE',  ( 0.000000000000000000, 265.0000000000000000, 0.000000000000000000 ) ) ;
#11113 = EDGE_CURVE ( 'NONE', #8974, #6884, #7353, .T. ) ;
#11114 = EDGE_LOOP ( 'NONE', ( #912, #12091, #8637 ) ) ;
#11115 = VECTOR ( 'NONE', #3733, 1000.000000000000114 ) ;
#11116 = FACE_OUTER_BOUND ( 'NONE', #984, .T. ) ;
#11117 = COLOUR_RGB ( '', 0.09019608, 0.27058824, 0.51372549) ;
#11118 = DIRECTION ( 'NONE',  ( 0.000000000000000000, 0.000000000000000000, 1.000000000000000000 ) ) ;
#11119 = ORIENTED_EDGE ( 'NONE', *, *, #1972, .F. ) ;
#11120 = CARTESIAN_POINT ( 'NONE',  ( 2.298097038856278918, 110.8750000000000000, -2.298097038856279806 ) ) ;
#11121 = DIRECTION ( 'NONE',  ( 0.000000000000000000, -0.4999999999999976685, 0.8660254037844399289 ) ) ;
#11122 = VERTEX_POINT ( 'NONE', #7532 ) ;
#11123 = CARTESIAN_POINT ( 'NONE',  ( -28.72281323269012532, 77.00000000000000000, 8.660254037844445918 ) ) ;
#11124 = CARTESIAN_POINT ( 'NONE',  ( 8.572527594031474570E-15, 62.00000000000000000, 70.00000000000001421 ) ) ;
#11125 = CARTESIAN_POINT ( 'NONE',  ( 2.708734125000000326, 112.3124999986344079, 0.000000000000000000 ) ) ;
#11126 = CARTESIAN_POINT ( 'NONE',  ( 2.708734124999999437, 113.4999999986344079, -1.121994411437820638 ) ) ;
#11127 = EDGE_CURVE ( 'NONE', #2311, #5671, #8209, .T. ) ;
#11128 = EDGE_CURVE ( 'NONE', #11256, #2522, #6419, .T. ) ;
#11129 = ORIENTED_EDGE ( 'NONE', *, *, #982, .F. ) ;
#11130 = DIRECTION ( 'NONE',  ( -1.000000000000000000, 0.000000000000000000, 0.000000000000000000 ) ) ;
#11131 = LINE ( 'NONE', #7395, #7535 ) ;
#11132 = CARTESIAN_POINT ( 'NONE',  ( 9.984215786548631399, 23.35566243268464603, 80.00000048127353125 ) ) ;
#11133 = EDGE_CURVE ( 'NONE', #632, #11972, #10205, .T. ) ;
#11134 = CARTESIAN_POINT ( 'NONE',  ( -9.726035167149685634, 24.78349364905394125, 80.00000000000000000 ) ) ;
#11135 = CARTESIAN_POINT ( 'NONE',  ( 7.344472908539098732, 24.78349364905406205, 80.00000000000000000 ) ) ;
#11136 = CARTESIAN_POINT ( 'NONE',  ( -16.19078112930547775, 31.03558258355681687, 73.23154106273423736 ) ) ;
#11137 = LINE ( 'NONE', #5285, #8785 ) ;
#11138 = CARTESIAN_POINT ( 'NONE',  ( 70.40913241174638415, 13.44666843646714405, -25.83788073351890802 ) ) ;
#11139 = CARTESIAN_POINT ( 'NONE',  ( 3.249999999999999556, 111.9374999999999858, -1.346194077712561610 ) ) ;
#11140 = DIRECTION ( 'NONE',  ( 0.000000000000000000, 0.000000000000000000, -1.000000000000000000 ) ) ;
#11141 = VECTOR ( 'NONE', #9762, 1000.000000000000114 ) ;
#11142 = CIRCLE ( 'NONE', #5776, 4.999999999999997335 ) ;
#11143 = CARTESIAN_POINT ( 'NONE',  ( 0.000000000000000000, 290.0000000000000568, 0.000000000000000000 ) ) ;
#11144 = VERTEX_POINT ( 'NONE', #12032 ) ;
#11145 = CARTESIAN_POINT ( 'NONE',  ( 6.000000000000000888, 62.00000000000000000, 60.00000000000002132 ) ) ;
#11146 = ADVANCED_FACE ( 'NONE', ( #7476 ), #810, .T. ) ;
#11147 = LINE ( 'NONE', #7412, #8642 ) ;
#11148 = EDGE_CURVE ( 'NONE', #4433, #1429, #4766, .T. ) ;
#11149 = CARTESIAN_POINT ( 'NONE',  ( 74.42783152987426831, 18.19891539281256598, -24.66728717810469362 ) ) ;
#11150 = EDGE_LOOP ( 'NONE', ( #3484, #6302, #4425, #1262 ) ) ;
#11151 = AXIS2_PLACEMENT_3D ( 'NONE', #6880, #11809, #6818 ) ;
#11152 = CARTESIAN_POINT ( 'NONE',  ( 0.000000000000000000, 165.5000000000000000, 0.000000000000000000 ) ) ;
#11153 = DIRECTION ( 'NONE',  ( -0.7071067811865455743, 0.7071067811865495711, 0.000000000000000000 ) ) ;
#11154 = EDGE_CURVE ( 'NONE', #9269, #7094, #12280, .T. ) ;
#11155 = EDGE_LOOP ( 'NONE', ( #3136, #11507, #6320, #1103 ) ) ;
#11156 = DIRECTION ( 'NONE',  ( -1.000000000000000000, -0.000000000000000000, -0.000000000000000000 ) ) ;
#11157 = CIRCLE ( 'NONE', #3779, 2.099999999999998312 ) ;
#11158 = AXIS2_PLACEMENT_3D ( 'NONE', #4590, #920, #6342 ) ;
#11159 = CIRCLE ( 'NONE', #7751, 40.00000000000000000 ) ;
#11160 = ORIENTED_EDGE ( 'NONE', *, *, #9499, .F. ) ;
#11161 = CARTESIAN_POINT ( 'NONE',  ( 0.000000000000000000, 50.00000000000000000, -75.00000000000001421 ) ) ;
#11162 = ORIENTED_EDGE ( 'NONE', *, *, #4103, .T. ) ;
#11163 = ORIENTED_EDGE ( 'NONE', *, *, #7214, .T. ) ;
#11164 = CARTESIAN_POINT ( 'NONE',  ( 2.500000000000000000, -1.178949249685214307, 2.042000000000001592 ) ) ;
#11165 = FACE_OUTER_BOUND ( 'NONE', #10482, .T. ) ;
#11166 = ORIENTED_EDGE ( 'NONE', *, *, #3756, .T. ) ;
#11167 =( NAMED_UNIT ( * ) PLANE_ANGLE_UNIT ( ) SI_UNIT ( $, .RADIAN. ) );
#11168 = CARTESIAN_POINT ( 'NONE',  ( -31.74999999999995737, 0.000000000000000000, 0.000000000000000000 ) ) ;
#11170 = CARTESIAN_POINT ( 'NONE',  ( -25.00000000000000000, 445.0000000000000568, -95.00000000000000000 ) ) ;
#11169 = AXIS2_PLACEMENT_3D ( 'NONE', #1403, #8991, #7196 ) ;
#11171 = PLANE ( 'NONE',  #833 ) ;
#11172 = COLOUR_RGB ( '', 0.66274510, 0.83137255, 0.94901961) ;
#11173 = EDGE_LOOP ( 'NONE', ( #7871, #3298, #9097, #9362 ) ) ;
#11174 = CARTESIAN_POINT ( 'NONE',  ( -1.121994411437820194, 114.2499999986344079, -2.708734124999999437 ) ) ;
#11175 = CARTESIAN_POINT ( 'NONE',  ( 165.0000000000011369, 225.0000000000000853, 25.00000000000000000 ) ) ;
#11176 = AXIS2_PLACEMENT_3D ( 'NONE', #7858, #9847, #3943 ) ;
#11177 = AXIS2_PLACEMENT_3D ( 'NONE', #9402, #3741, #11419 ) ;
#11178 = EDGE_LOOP ( 'NONE', ( #10935, #1361, #4351, #3302 ) ) ;
#11179 = CARTESIAN_POINT ( 'NONE',  ( 11.80921887069467324, 29.75000000000018474, 80.00000000000000000 ) ) ;
#11180 = CARTESIAN_POINT ( 'NONE',  ( 71.39985347493268364, 48.95609667407049415, 22.96547907468804084 ) ) ;
#11181 = ORIENTED_EDGE ( 'NONE', *, *, #5390, .F. ) ;
#11182 = CARTESIAN_POINT ( 'NONE',  ( -1.346194077712573822, 112.3125000000000000, 3.249999999999985789 ) ) ;
#11183 = DIRECTION ( 'NONE',  ( 0.000000000000000000, 1.000000000000000000, 0.000000000000000000 ) ) ;
#11184 = ORIENTED_EDGE ( 'NONE', *, *, #4793, .F. ) ;
#11185 = DIRECTION ( 'NONE',  ( 0.000000000000000000, 0.000000000000000000, 1.000000000000000000 ) ) ;
#11186 = DIRECTION ( 'NONE',  ( 0.8660254037844365982, -0.5000000000000036637, 0.000000000000000000 ) ) ;
#11187 = CARTESIAN_POINT ( 'NONE',  ( 11.80921887069467324, 29.75000000000018474, 79.50000000000000000 ) ) ;
#11188 = AXIS2_PLACEMENT_3D ( 'NONE', #5160, #4092, #1290 ) ;
#11189 = ADVANCED_FACE ( 'NONE', ( #11095 ), #7417, .F. ) ;
#11190 = CARTESIAN_POINT ( 'NONE',  ( -4.975863863883684959E-16, 111.3124999986344079, -2.708734124999999882 ) ) ;
#11191 = VECTOR ( 'NONE', #11485, 1000.000000000000000 ) ;
#11192 = ORIENTED_EDGE ( 'NONE', *, *, #5181, .T. ) ;
#11193 = ORIENTED_EDGE ( 'NONE', *, *, #5852, .T. ) ;
#11194 = PRESENTATION_STYLE_ASSIGNMENT (( #1718 ) ) ;
#11195 = LINE ( 'NONE', #10118, #5460 ) ;
#11196 = CARTESIAN_POINT ( 'NONE',  ( 0.000000000000000000, 109.0000000000000000, 0.000000000000000000 ) ) ;
#11197 = EDGE_CURVE ( 'NONE', #4302, #10953, #2770, .T. ) ;
#11198 = FACE_OUTER_BOUND ( 'NONE', #3069, .T. ) ;
#11199 = CARTESIAN_POINT ( 'NONE',  ( 11.80921887069467324, 29.75000000000018474, 80.00000000000000000 ) ) ;
#11200 = EDGE_CURVE ( 'NONE', #5052, #11037, #4571, .T. ) ;
#11201 = CARTESIAN_POINT ( 'NONE',  ( -27.94372984915577618, 86.14533704847946183, -11.47449158599561692 ) ) ;
#11202 = LINE ( 'NONE', #2535, #4912 ) ;
#11203 = CYLINDRICAL_SURFACE ( 'NONE', #3220, 2.649999999999993694 ) ;
#11204 = EDGE_LOOP ( 'NONE', ( #2278, #1274, #4233, #8842 ) ) ;
#11205 = CARTESIAN_POINT ( 'NONE',  ( 3.249999999999999556, 113.9374999999999858, -1.346194077712561610 ) ) ;
#11206 = B_SPLINE_CURVE_WITH_KNOTS ( 'NONE', 3,
 ( #8285, #9214, #6494, #10281 ),
 .UNSPECIFIED., .F., .F.,
 ( 4, 4 ),
 ( 0.000000000000000000, 0.002955678282115210744 ),
 .UNSPECIFIED. ) ;
#11207 = CARTESIAN_POINT ( 'NONE',  ( 45.35898384862240107, 67.00000000000008527, -25.98076211353315657 ) ) ;
#11208 = CIRCLE ( 'NONE', #7422, 3.399999999999999911 ) ;
#11209 = FACE_OUTER_BOUND ( 'NONE', #7046, .T. ) ;
#11210 = ORIENTED_EDGE ( 'NONE', *, *, #6412, .T. ) ;
#11211 = ADVANCED_FACE ( 'NONE', ( #3548 ), #9202, .F. ) ;
#11212 = EDGE_CURVE ( 'NONE', #10746, #11226, #12338, .T. ) ;
#11213 = DIRECTION ( 'NONE',  ( -0.000000000000000000, -1.000000000000000000, -0.000000000000000000 ) ) ;
#11214 = CARTESIAN_POINT ( 'NONE',  ( 0.2500000000000002220, 5.204748896376250699E-16, -4.250000000000000000 ) ) ;
#11215 = CARTESIAN_POINT ( 'NONE',  ( 0.000000000000000000, 115.0000000000000000, 9.999999999999998224 ) ) ;
#11216 = ORIENTED_EDGE ( 'NONE', *, *, #608, .F. ) ;
#11217 = AXIS2_PLACEMENT_3D ( 'NONE', #1486, #10832, #11784 ) ;
#11218 = DIRECTION ( 'NONE',  ( 0.000000000000000000, 0.000000000000000000, 1.000000000000000000 ) ) ;
#11219 = DIRECTION ( 'NONE',  ( 0.000000000000000000, 0.000000000000000000, 1.000000000000000000 ) ) ;
#11220 = VERTEX_POINT ( 'NONE', #8639 ) ;
#11221 = DIRECTION ( 'NONE',  ( 0.000000000000000000, 0.000000000000000000, 1.000000000000000000 ) ) ;
#11222 = VECTOR ( 'NONE', #10514, 1000.000000000000000 ) ;
#11223 = ORIENTED_EDGE ( 'NONE', *, *, #8750, .F. ) ;
#11224 = DIRECTION ( 'NONE',  ( 0.000000000000000000, 0.000000000000000000, 1.000000000000000000 ) ) ;
#11226 = VERTEX_POINT ( 'NONE', #11469 ) ;
#11225 = CARTESIAN_POINT ( 'NONE',  ( 3.980102097228898231E-16, 110.0000000000000000, -3.250000000000000444 ) ) ;
#11227 = ORIENTED_EDGE ( 'NONE', *, *, #5725, .F. ) ;
#11228 = ADVANCED_BREP_SHAPE_REPRESENTATION ( '', ( #4709, #1612 ), #3176 ) ;
#11229 = FACE_OUTER_BOUND ( 'NONE', #4813, .T. ) ;
#11230 = CARTESIAN_POINT ( 'NONE',  ( -29.94260118448502794, 78.56931597186009242, 5.428213010295147356 ) ) ;
#11231 = ORIENTED_EDGE ( 'NONE', *, *, #1926, .T. ) ;
#11232 = CARTESIAN_POINT ( 'NONE',  ( 0.000000000000000000, 0.000000000000000000, 0.000000000000000000 ) ) ;
#11233 = FACE_OUTER_BOUND ( 'NONE', #11880, .T. ) ;
#11234 = CARTESIAN_POINT ( 'NONE',  ( 25.00000000000000000, 445.0000000000000568, -90.00000000000000000 ) ) ;
#11235 = DIRECTION ( 'NONE',  ( -0.000000000000000000, -1.000000000000000000, -0.000000000000000000 ) ) ;
#11236 = CIRCLE ( 'NONE', #3857, 12.99999999999999822 ) ;
#11237 = VECTOR ( 'NONE', #7545, 999.9999999999998863 ) ;
#11238 = ORIENTED_EDGE ( 'NONE', *, *, #8544, .T. ) ;
#11239 = CARTESIAN_POINT ( 'NONE',  ( -4.975863863883684959E-16, 113.3124999986344079, -2.708734124999999882 ) ) ;
#11240 = LINE ( 'NONE', #5568, #1814 ) ;
#11241 =( REPRESENTATION_RELATIONSHIP ('NONE','NONE', #3713, #10952 ) REPRESENTATION_RELATIONSHIP_WITH_TRANSFORMATION ( #4734 )SHAPE_REPRESENTATION_RELATIONSHIP( ) );
#11242 = EDGE_CURVE ( 'NONE', #5677, #9755, #10641, .T. ) ;
#11243 = B_SPLINE_CURVE_WITH_KNOTS ( 'NONE', 3,
 ( #12203, #7459, #4332, #1540 ),
 .UNSPECIFIED., .F., .F.,
 ( 4, 4 ),
 ( 0.0009573067811866343675, 0.001207306781186544276 ),
 .UNSPECIFIED. ) ;
#11244 = ORIENTED_EDGE ( 'NONE', *, *, #10225, .F. ) ;
#11245 = CARTESIAN_POINT ( 'NONE',  ( 1.224646799147353059E-15, 165.0000000000000000, 9.999999999999998224 ) ) ;
#11246 = CARTESIAN_POINT ( 'NONE',  ( 69.89773400907223788, 44.39854272105920785, 27.19132888315843033 ) ) ;
#11247 = ORIENTED_EDGE ( 'NONE', *, *, #9614, .T. ) ;
#11248 = AXIS2_PLACEMENT_3D ( 'NONE', #10190, #4463, #11011 ) ;
#11249 = DIRECTION ( 'NONE',  ( 0.000000000000000000, 1.000000000000000000, 0.000000000000000000 ) ) ;
#11250 = DIRECTION ( 'NONE',  ( 0.000000000000000000, 0.000000000000000000, 1.000000000000000000 ) ) ;
#11251 = ORIENTED_EDGE ( 'NONE', *, *, #5344, .T. ) ;
#11252 = CARTESIAN_POINT ( 'NONE',  ( 89.80805993797383735, 275.0000000000000000, 81.82974571984303225 ) ) ;
#11253 = CARTESIAN_POINT ( 'NONE',  ( -6.407287480251391720, 21.46474596215567487, 79.50000000000000000 ) ) ;
#11254 = CARTESIAN_POINT ( 'NONE',  ( 2.708734124999999882, 112.6249999986343937, 1.121994411437818862 ) ) ;
#11255 = B_SPLINE_CURVE_WITH_KNOTS ( 'NONE', 3,
 ( #9782, #3186, #7110, #6986, #10785, #9841, #2366, #4121, #1257, #5184, #10906, #7909, #9025, #9905, #11799, #2309 ),
 .UNSPECIFIED., .F., .F.,
 ( 4, 2, 2, 2, 2, 2, 2, 4 ),
 ( 0.000000000000000000, 0.001377885821436785046, 0.002066828732155181255, 0.002755771642873577464, 0.003444714553591973240, 0.004133657464310369449, 0.004822600375028765658, 0.005511543285747161867 ),
 .UNSPECIFIED. ) ;
#11256 = VERTEX_POINT ( 'NONE', #2046 ) ;
#11257 = VERTEX_POINT ( 'NONE', #3921 ) ;
#11258 = TOROIDAL_SURFACE ( 'NONE', #7467, 25.00000000000000000, 8.000000000000000000 ) ;
#11259 = ORIENTED_EDGE ( 'NONE', *, *, #376, .F. ) ;
#11260 = B_SPLINE_CURVE_WITH_KNOTS ( 'NONE', 3,
 ( #620, #9833, #1557, #3367, #3238, #3177, #1368, #4171, #10901, #430, #9898, #11792, #2425, #8956, #7227, #9139 ),
 .UNSPECIFIED., .F., .F.,
 ( 4, 2, 2, 2, 2, 2, 2, 4 ),
 ( 0.000000000000000000, 0.001377885821436793719, 0.002066828732155186893, 0.002755771642873580500, 0.003444714553591973673, 0.004133657464310366847, 0.004822600375028760454, 0.005511543285747163602 ),
 .UNSPECIFIED. ) ;
#11261 = VECTOR ( 'NONE', #3326, 1000.000000000000000 ) ;
#11262 = ADVANCED_FACE ( 'NONE', ( #7775 ), #8576, .T. ) ;
#11263 = LINE ( 'NONE', #4580, #8028 ) ;
#11264 = EDGE_CURVE ( 'NONE', #3440, #8327, #7939, .T. ) ;
#11265 = FACE_OUTER_BOUND ( 'NONE', #11114, .T. ) ;
#11266 = CARTESIAN_POINT ( 'NONE',  ( -14.19078112930532853, 30.25000000000008882, 79.50000000000000000 ) ) ;
#11267 = CIRCLE ( 'NONE', #5292, 3.399999999999999911 ) ;
#11268 = DIRECTION ( 'NONE',  ( 0.000000000000000000, 1.000000000000000000, 0.000000000000000000 ) ) ;
#11269 = DIRECTION ( 'NONE',  ( -0.000000000000000000, -1.000000000000000000, -0.000000000000000000 ) ) ;
#11270 = CARTESIAN_POINT ( 'NONE',  ( -7.093000575290183463, 43.82875375259622075, 74.67028158002766247 ) ) ;
#11271 = CARTESIAN_POINT ( 'NONE',  ( 0.000000000000000000, 290.0000000000000568, 0.000000000000000000 ) ) ;
#11272 = CARTESIAN_POINT ( 'NONE',  ( 0.000000000000000000, 115.0000000000000142, -17.00000000000000000 ) ) ;
#11273 = VECTOR ( 'NONE', #960, 1000.000000000000000 ) ;
#11274 = EDGE_CURVE ( 'NONE', #8994, #10639, #1982, .T. ) ;
#11275 = ADVANCED_FACE ( 'NONE', ( #5792 ), #11402, .F. ) ;
#11276 = CARTESIAN_POINT ( 'NONE',  ( 2.298097038856279806, 112.9999999972688158, 2.298097038856279806 ) ) ;
#11277 = VECTOR ( 'NONE', #10528, 1000.000000000000000 ) ;
#11278 = DIRECTION ( 'NONE',  ( 0.5000000000000036637, 0.8660254037844364872, 0.000000000000000000 ) ) ;
#11279 = EDGE_LOOP ( 'NONE', ( #9859, #9027, #3546, #3330 ) ) ;
#11280 = DIRECTION ( 'NONE',  ( 1.000000000000000000, 0.000000000000000000, 0.000000000000000000 ) ) ;
#11281 = EDGE_CURVE ( 'NONE', #3270, #1995, #8138, .T. ) ;
#11282 = LINE ( 'NONE', #9262, #2095 ) ;
#11283 = DIRECTION ( 'NONE',  ( 0.000000000000000000, -0.8660254037844405950, -0.4999999999999965028 ) ) ;
#11284 = ORIENTED_EDGE ( 'NONE', *, *, #2567, .T. ) ;
#11285 = CARTESIAN_POINT ( 'NONE',  ( -75.98513253586240523, 275.0000000000000000, 72.46557550663233371 ) ) ;
#11286 = COLOUR_RGB ( '', 0.40784314, 0.44705882, 0.49803922) ;
#11287 = CARTESIAN_POINT ( 'NONE',  ( 0.000000000000000000, 260.0000000000000000, 0.000000000000000000 ) ) ;
#11288 = VERTEX_POINT ( 'NONE', #9698 ) ;
#11289 = CARTESIAN_POINT ( 'NONE',  ( 2.388061258337338939E-15, 127.0000000000000000, -17.00000000000000000 ) ) ;
#11290 = VECTOR ( 'NONE', #1601, 1000.000000000000000 ) ;
#11291 = EDGE_CURVE ( 'NONE', #5123, #5829, #11946, .T. ) ;
#11292 = EDGE_CURVE ( 'NONE', #8492, #4699, #8704, .T. ) ;
#11293 = EDGE_LOOP ( 'NONE', ( #10207, #8811, #7757, #177 ) ) ;
#11294 = DIRECTION ( 'NONE',  ( 0.000000000000000000, 0.000000000000000000, 1.000000000000000000 ) ) ;
#11295 = CARTESIAN_POINT ( 'NONE',  ( 0.000000000000000000, 110.0000000000000000, 0.000000000000000000 ) ) ;
#11296 = ORIENTED_EDGE ( 'NONE', *, *, #11200, .F. ) ;
#11297 = AXIS2_PLACEMENT_3D ( 'NONE', #5330, #11186, #5578 ) ;
#11298 = CARTESIAN_POINT ( 'NONE',  ( -31.12930703771215235, 75.68563247576862807, 7.901403593909491541 ) ) ;
#11299 = ORIENTED_EDGE ( 'NONE', *, *, #9421, .F. ) ;
#11300 = FACE_OUTER_BOUND ( 'NONE', #1616, .T. ) ;
#11301 = DIRECTION ( 'NONE',  ( 0.000000000000000000, 0.000000000000000000, 1.000000000000000000 ) ) ;
#11302 = LINE ( 'NONE', #5564, #223 ) ;
#11303 = ORIENTED_EDGE ( 'NONE', *, *, #12194, .F. ) ;
#11304 = CARTESIAN_POINT ( 'NONE',  ( 1.121994411437818862, 110.4999999986344079, 2.708734125000000326 ) ) ;
#11305 = VERTEX_POINT ( 'NONE', #9575 ) ;
#11306 = CARTESIAN_POINT ( 'NONE',  ( 165.0000000000011369, 35.00000000000004974, -25.00000000000000000 ) ) ;
#11307 = CARTESIAN_POINT ( 'NONE',  ( -15.13458840481166590, 24.44672303875686481, 73.45739858620734708 ) ) ;
#11308 = ORIENTED_EDGE ( 'NONE', *, *, #140, .F. ) ;
#11309 = CARTESIAN_POINT ( 'NONE',  ( 0.000000000000000000, 115.0000000000000000, 3.399999999999999911 ) ) ;
#11310 = CARTESIAN_POINT ( 'NONE',  ( 72.61843774138908714, 45.00000000000009948, 18.75000000000000711 ) ) ;
#11311 = ORIENTED_EDGE ( 'NONE', *, *, #10068, .F. ) ;
#11312 = EDGE_CURVE ( 'NONE', #8405, #7265, #5972, .T. ) ;
#11313 = ADVANCED_FACE ( 'NONE', ( #7834 ), #10520, .F. ) ;
#11314 = CARTESIAN_POINT ( 'NONE',  ( -25.00000000000000000, 445.0000000000000568, -90.00000000000000000 ) ) ;
#11315 = CARTESIAN_POINT ( 'NONE',  ( 0.000000000000000000, 127.0000000000000000, 17.00000000000000000 ) ) ;
#11316 = CARTESIAN_POINT ( 'NONE',  ( 1.346194077712559833, 114.6874999972688158, -3.250000000000000000 ) ) ;
#11317 = CARTESIAN_POINT ( 'NONE',  ( -4.975863863883684959E-16, 111.3124999986344079, -2.708734124999999882 ) ) ;
#11318 = EDGE_CURVE ( 'NONE', #6826, #4551, #991, .T. ) ;
#11319 = ORIENTED_EDGE ( 'NONE', *, *, #8599, .T. ) ;
#11320 = VECTOR ( 'NONE', #6727, 1000.000000000000000 ) ;
#11321 = PRESENTATION_STYLE_ASSIGNMENT (( #1900 ) ) ;
#11322 = DIRECTION ( 'NONE',  ( 0.000000000000000000, 0.000000000000000000, 1.000000000000000000 ) ) ;
#11323 = VERTEX_POINT ( 'NONE', #6909 ) ;
#11324 = DIRECTION ( 'NONE',  ( 7.011174048739587977E-15, 1.000000000000000000, 0.000000000000000000 ) ) ;
#11325 = DIRECTION ( 'NONE',  ( 0.000000000000000000, 1.000000000000000000, 0.000000000000000000 ) ) ;
#11326 = CARTESIAN_POINT ( 'NONE',  ( 0.000000000000000000, 115.0000000000000142, 0.000000000000000000 ) ) ;
#11327 = CONICAL_SURFACE ( 'NONE', #3748, 3.399999999999999911, 1.029744258676658974 ) ;
#11328 = FACE_OUTER_BOUND ( 'NONE', #1390, .T. ) ;
#11329 =( GEOMETRIC_REPRESENTATION_CONTEXT ( 3 ) GLOBAL_UNCERTAINTY_ASSIGNED_CONTEXT ( ( #1912 ) ) GLOBAL_UNIT_ASSIGNED_CONTEXT ( ( #3561, #11167, #10341 ) ) REPRESENTATION_CONTEXT ( 'NONE', 'WORKASPACE' ) );
#11330 = ORIENTED_EDGE ( 'NONE', *, *, #12207, .F. ) ;
#11331 = FACE_OUTER_BOUND ( 'NONE', #574, .T. ) ;
#11332 = CARTESIAN_POINT ( 'NONE',  ( 74.16874958671132845, 40.33405953496801999, -24.99164682819347760 ) ) ;
#11333 = EDGE_LOOP ( 'NONE', ( #7371, #6759 ) ) ;
#11334 = EDGE_CURVE ( 'NONE', #5535, #3208, #2174, .T. ) ;
#11335 = CARTESIAN_POINT ( 'NONE',  ( -11.19078112930532498, 30.25000000000005684, 79.50000000000000000 ) ) ;
#11336 = FACE_OUTER_BOUND ( 'NONE', #2945, .T. ) ;
#11337 = CARTESIAN_POINT ( 'NONE',  ( 70.88237045016090576, 18.32754774912132234, -24.73035864412310758 ) ) ;
#11338 = ORIENTED_EDGE ( 'NONE', *, *, #7969, .T. ) ;
#11339 = DIRECTION ( 'NONE',  ( -1.000000000000000000, 0.000000000000000000, 0.000000000000000000 ) ) ;
#11340 = CARTESIAN_POINT ( 'NONE',  ( 9.942549119892413856, 23.28349364905404428, 79.50000000000000000 ) ) ;
#11341 = ADVANCED_FACE ( 'NONE', ( #7592 ), #5074, .F. ) ;
#11342 = AXIS2_PLACEMENT_3D ( 'NONE', #6721, #6782, #11592 ) ;
#11343 = AXIS2_PLACEMENT_3D ( 'NONE', #1013, #3003, #3064 ) ;
#11344 = ORIENTED_EDGE ( 'NONE', *, *, #214, .F. ) ;
#11345 = DIRECTION ( 'NONE',  ( 1.000000000000000000, -0.000000000000000000, 6.938893903907228378E-17 ) ) ;
#11346 = VERTEX_POINT ( 'NONE', #6466 ) ;
#11347 = CARTESIAN_POINT ( 'NONE',  ( 1.163414459189985959E-14, 265.0000000000000000, -95.00000000000002842 ) ) ;
#11348 = CIRCLE ( 'NONE', #5585, 5.000000000000000888 ) ;
#11349 = CYLINDRICAL_SURFACE ( 'NONE', #658, 15.00000000000000000 ) ;
#11350 = VERTEX_POINT ( 'NONE', #3828 ) ;
#11351 = DIRECTION ( 'NONE',  ( 0.000000000000000000, 0.000000000000000000, 1.000000000000000000 ) ) ;
#11352 = VECTOR ( 'NONE', #5012, 1000.000000000000114 ) ;
#11353 = EDGE_LOOP ( 'NONE', ( #2122, #4269, #6011 ) ) ;
#11354 = EDGE_CURVE ( 'NONE', #7018, #1569, #3770, .T. ) ;
#11355 = DIRECTION ( 'NONE',  ( 1.000000000000000000, 0.000000000000000000, 0.000000000000000000 ) ) ;
#11356 = ADVANCED_FACE ( 'NONE', ( #7627 ), #11081, .T. ) ;
#11357 = PLANE ( 'NONE',  #11836 ) ;
#11358 = DIRECTION ( 'NONE',  ( -0.2207553928441736979, 0.8446598678744383637, 0.4876646020909772838 ) ) ;
#11359 = CARTESIAN_POINT ( 'NONE',  ( 140.0000000000011369, 230.0000000000000853, -19.99999999999999645 ) ) ;
#11360 = VERTEX_POINT ( 'NONE', #325 ) ;
#11361 = CARTESIAN_POINT ( 'NONE',  ( -2.708734124999999882, 113.9999999986343937, 1.121994411437818862 ) ) ;
#11362 = DIRECTION ( 'NONE',  ( 0.000000000000000000, -1.000000000000000000, 0.000000000000000000 ) ) ;
#11363 = EDGE_CURVE ( 'NONE', #9072, #9665, #3173, .T. ) ;
#11364 = EDGE_LOOP ( 'NONE', ( #6113, #3168, #8063, #1060, #9057 ) ) ;
#11365 = CARTESIAN_POINT ( 'NONE',  ( 1.408343819019456413E-14, 340.0000000000000000, 115.0000000000000284 ) ) ;
#11366 = CARTESIAN_POINT ( 'NONE',  ( -1.190781129305471087, 30.00000000000008882, 80.00000000000000000 ) ) ;
#11367 =( BOUNDED_CURVE ( )  B_SPLINE_CURVE ( 2, ( #5678, #5923, #10592, #239, #9520, #8713, #5740, #7543, #1933 ),
 .UNSPECIFIED., .F., .T. ) 
 B_SPLINE_CURVE_WITH_KNOTS ( ( 3, 2, 2, 2, 3 ),
 ( 0.06250000000000005551, 0.09375000000000008327, 0.1250000000000001110, 0.1562500000000001388, 0.1875000000000001665 ),
 .UNSPECIFIED. ) 
 CURVE ( )  GEOMETRIC_REPRESENTATION_ITEM ( )  RATIONAL_B_SPLINE_CURVE ( ( 0.9999999999999998890, 0.9238795325112868495, 1.000000000000000000, 0.9238795325112867385, 1.000000000000000000, 0.9238795325112867385, 1.000000000000000000, 0.9238795325112862944, 1.000000000000000444 ) ) 
 REPRESENTATION_ITEM ( '' )  );
#11368 = ORIENTED_EDGE ( 'NONE', *, *, #903, .F. ) ;
#11369 = DIRECTION ( 'NONE',  ( 0.000000000000000000, 1.000000000000000000, 0.000000000000000000 ) ) ;
#11370 = DIRECTION ( 'NONE',  ( 0.000000000000000000, 0.000000000000000000, -1.000000000000000000 ) ) ;
#11371 = VERTEX_POINT ( 'NONE', #11562 ) ;
#11372 = DIRECTION ( 'NONE',  ( -1.040834085586083310E-14, -1.000000000000000000, 0.000000000000000000 ) ) ;
#11373 = FACE_OUTER_BOUND ( 'NONE', #4537, .T. ) ;
#11374 = LINE ( 'NONE', #12, #7952 ) ;
#11375 = DIRECTION ( 'NONE',  ( 1.564230817409691233E-15, 0.000000000000000000, -1.000000000000000000 ) ) ;
#11376 = ORIENTED_EDGE ( 'NONE', *, *, #5654, .T. ) ;
#11377 = CIRCLE ( 'NONE', #9765, 95.00000000000002842 ) ;
#11378 = ADVANCED_FACE ( 'NONE', ( #4075 ), #3016, .T. ) ;
#11379 = EDGE_LOOP ( 'NONE', ( #258, #450, #1381, #4730 ) ) ;
#11380 = PRODUCT_RELATED_PRODUCT_CATEGORY ( 'part', '', ( #11777 ) ) ;
#11381 = ADVANCED_FACE ( 'NONE', ( #1086 ), #5079, .T. ) ;
#11382 = FILL_AREA_STYLE_COLOUR ( '', #10629 ) ;
#11383 = FACE_OUTER_BOUND ( 'NONE', #3233, .T. ) ;
#11384 = ORIENTED_EDGE ( 'NONE', *, *, #2427, .T. ) ;
#11385 = AXIS2_PLACEMENT_3D ( 'NONE', #3375, #10151, #7173 ) ;
#11386 = DIRECTION ( 'NONE',  ( -0.7071067811865447972, 0.7071067811865503483, 0.000000000000000000 ) ) ;
#11387 = LINE ( 'NONE', #8437, #9356 ) ;
#11388 = VECTOR ( 'NONE', #665, 1000.000000000000000 ) ;
#11389 = CARTESIAN_POINT ( 'NONE',  ( -34.31149098582250190, 75.26794919243110371, 7.660254037844446806 ) ) ;
#11390 = CARTESIAN_POINT ( 'NONE',  ( 0.000000000000000000, 265.0000000000000000, 0.000000000000000000 ) ) ;
#11391 = DIRECTION ( 'NONE',  ( -0.000000000000000000, -1.000000000000000000, -0.000000000000000000 ) ) ;
#11392 = VECTOR ( 'NONE', #2717, 1000.000000000000000 ) ;
#11393 = EDGE_CURVE ( 'NONE', #7317, #10706, #11740, .T. ) ;
#11394 = UNCERTAINTY_MEASURE_WITH_UNIT (LENGTH_MEASURE( 1.000000000000000082E-05 ), #967, 'distance_accuracy_value', 'NONE');
#11395 = CARTESIAN_POINT ( 'NONE',  ( 71.59624044336383974, 44.46613403158139022, -22.48149205125841377 ) ) ;
#11396 = EDGE_LOOP ( 'NONE', ( #4150, #2178, #8155, #11533 ) ) ;
#11397 = DIRECTION ( 'NONE',  ( -0.000000000000000000, -0.000000000000000000, 1.000000000000000000 ) ) ;
#11398 = CARTESIAN_POINT ( 'NONE',  ( -20.00000000000000355, 65.00000000000000000, -57.08203932499370836 ) ) ;
#11399 = CARTESIAN_POINT ( 'NONE',  ( 71.05921646411502479, 17.18492608871972394, -24.19824146092191697 ) ) ;
#11400 = ORIENTED_EDGE ( 'NONE', *, *, #12329, .T. ) ;
#11401 = DIRECTION ( 'NONE',  ( -1.000000000000000000, 8.326672684688666165E-15, 0.000000000000000000 ) ) ;
#11402 = CYLINDRICAL_SURFACE ( 'NONE', #9730, 2.099999999999993427 ) ;
#11403 = VECTOR ( 'NONE', #1840, 1000.000000000000000 ) ;
#11404 = ORIENTED_EDGE ( 'NONE', *, *, #9054, .F. ) ;
#11405 = DIRECTION ( 'NONE',  ( -0.8660254037844410391, -0.4999999999999958367, 0.000000000000000000 ) ) ;
#11406 = EDGE_LOOP ( 'NONE', ( #10319, #2428, #11238, #11641 ) ) ;
#11407 = AXIS2_PLACEMENT_3D ( 'NONE', #10907, #4424, #3494 ) ;
#11408 = EDGE_CURVE ( 'NONE', #5372, #10506, #2256, .T. ) ;
#11409 = DIRECTION ( 'NONE',  ( -1.734723475976805517E-15, 1.000000000000000000, -0.000000000000000000 ) ) ;
#11410 = CARTESIAN_POINT ( 'NONE',  ( 0.000000000000000000, 50.00000000000000000, -70.00000000000001421 ) ) ;
#11411 = ORIENTED_EDGE ( 'NONE', *, *, #5064, .T. ) ;
#11412 = ADVANCED_FACE ( 'NONE', ( #4889 ), #8677, .T. ) ;
#11413 = DIRECTION ( 'NONE',  ( 1.000000000000000000, 0.000000000000000000, 0.000000000000000000 ) ) ;
#11414 = CARTESIAN_POINT ( 'NONE',  ( 165.0000000000011369, 225.0000000000000853, 20.00000000000000000 ) ) ;
#11415 = ORIENTED_EDGE ( 'NONE', *, *, #2349, .T. ) ;
#11416 = APPLICATION_PROTOCOL_DEFINITION ( 'draft international standard', 'automotive_design', 1998, #6138 ) ;
#11417 = CARTESIAN_POINT ( 'NONE',  ( -1.190781129305471087, 30.00000000000008882, 78.00000000000000000 ) ) ;
#11418 = DIRECTION ( 'NONE',  ( 0.000000000000000000, 0.000000000000000000, -1.000000000000000000 ) ) ;
#11419 = DIRECTION ( 'NONE',  ( 0.000000000000000000, 0.000000000000000000, 1.000000000000000000 ) ) ;
#11420 = ORIENTED_EDGE ( 'NONE', *, *, #7466, .T. ) ;
#11421 = CARTESIAN_POINT ( 'NONE',  ( 1.658621287961228320E-16, 111.8124999986344079, 2.708734124999999882 ) ) ;
#11422 = CARTESIAN_POINT ( 'NONE',  ( -2.298097038856279806, 113.4999999972688158, -2.298097038856279362 ) ) ;
#11423 = VERTEX_POINT ( 'NONE', #8735 ) ;
#11424 = EDGE_CURVE ( 'NONE', #10397, #875, #9750, .T. ) ;
#11425 = CARTESIAN_POINT ( 'NONE',  ( 0.000000000000000000, 340.0000000000000000, -34.99999999999999289 ) ) ;
#11426 = CARTESIAN_POINT ( 'NONE',  ( 71.75476781871510923, 49.45246612713112455, 21.82544253889693309 ) ) ;
#11427 = ORIENTED_EDGE ( 'NONE', *, *, #6712, .F. ) ;
#11428 = DIRECTION ( 'NONE',  ( -1.000000000000000000, 0.000000000000000000, 0.000000000000000000 ) ) ;
#11429 = CARTESIAN_POINT ( 'NONE',  ( 69.85318522031717237, 15.89659164372772970, 27.30472166927799194 ) ) ;
#11430 = ORIENTED_EDGE ( 'NONE', *, *, #7229, .T. ) ;
#11431 = VECTOR ( 'NONE', #7203, 1000.000000000000000 ) ;
#11432 = AXIS2_PLACEMENT_3D ( 'NONE', #8528, #3933, #10596 ) ;
#11433 = ADVANCED_FACE ( 'NONE', ( #8796 ), #7748, .T. ) ;
#11434 = DIRECTION ( 'NONE',  ( 0.000000000000000000, 0.000000000000000000, -1.000000000000000000 ) ) ;
#11435 = CARTESIAN_POINT ( 'NONE',  ( -8.500000000000000000, 122.5000000000000000, -7.483314773547880883 ) ) ;
#11436 = PLANE ( 'NONE',  #10143 ) ;
#11437 = CARTESIAN_POINT ( 'NONE',  ( -3.250000000000000444, 110.5000000000000000, 3.980102097228898231E-16 ) ) ;
#11438 = CARTESIAN_POINT ( 'NONE',  ( 1.658621287961228320E-16, 112.8124999986344079, 2.708734124999999882 ) ) ;
#11439 = VERTEX_POINT ( 'NONE', #10615 ) ;
#11440 = EDGE_CURVE ( 'NONE', #11305, #3755, #12294, .T. ) ;
#11441 = EDGE_CURVE ( 'NONE', #44, #12227, #4011, .T. ) ;
#11442 = VECTOR ( 'NONE', #8239, 1000.000000000000227 ) ;
#11443 =( BOUNDED_CURVE ( )  B_SPLINE_CURVE ( 2, ( #8958, #5124, #7106, #9901, #4297, #9962, #3303, #5180, #8151 ),
 .UNSPECIFIED., .F., .F. ) 
 B_SPLINE_CURVE_WITH_KNOTS ( ( 3, 2, 2, 2, 3 ),
 ( 0.8125000000000006661, 0.8437500000000006661, 0.8750000000000006661, 0.9062500000000007772, 0.9375000000000007772 ),
 .UNSPECIFIED. ) 
 CURVE ( )  GEOMETRIC_REPRESENTATION_ITEM ( )  RATIONAL_B_SPLINE_CURVE ( ( 0.9999999999999983347, 0.9238795325112884038, 1.000000000000000000, 0.9238795325112867385, 1.000000000000000000, 0.9238795325112867385, 1.000000000000000000, 0.9238795325112848511, 1.000000000000001998 ) ) 
 REPRESENTATION_ITEM ( '' )  );
#11444 = VECTOR ( 'NONE', #3300, 1000.000000000000114 ) ;
#11445 = ORIENTED_EDGE ( 'NONE', *, *, #10228, .T. ) ;
#11446 = FILL_AREA_STYLE ('',( #11382 ) ) ;
#11447 = CARTESIAN_POINT ( 'NONE',  ( 4.953017525665607934, 43.69200144738164937, 74.83745130172235349 ) ) ;
#11448 = VERTEX_POINT ( 'NONE', #5140 ) ;
#11449 = CARTESIAN_POINT ( 'NONE',  ( 30.00100000000000122, 85.26794919243110371, -9.660254037844429931 ) ) ;
#11450 = CARTESIAN_POINT ( 'NONE',  ( -25.00000000000000000, 450.0000000000000568, -14.99999999999999289 ) ) ;
#11451 = DIRECTION ( 'NONE',  ( -0.000000000000000000, -1.000000000000000000, -0.000000000000000000 ) ) ;
#11452 = DIRECTION ( 'NONE',  ( -0.000000000000000000, -1.000000000000000000, -0.000000000000000000 ) ) ;
#11453 = AXIS2_PLACEMENT_3D ( 'NONE', #10018, #6917, #5116 ) ;
#11454 = ORIENTED_EDGE ( 'NONE', *, *, #1655, .F. ) ;
#11455 = AXIS2_PLACEMENT_3D ( 'NONE', #6239, #3372, #5306 ) ;
#11456 = PRESENTATION_STYLE_ASSIGNMENT (( #9624 ) ) ;
#11457 = CIRCLE ( 'NONE', #7869, 110.0000000000000284 ) ;
#11458 = FACE_OUTER_BOUND ( 'NONE', #11517, .T. ) ;
#11459 = AXIS2_PLACEMENT_3D ( 'NONE', #10476, #3056, #5744 ) ;
#11460 = CYLINDRICAL_SURFACE ( 'NONE', #12064, 44.99999999999999289 ) ;
#11461 = CYLINDRICAL_SURFACE ( 'NONE', #2655, 5.000000000000000000 ) ;
#11462 = CARTESIAN_POINT ( 'NONE',  ( 77.45966692414833688, 50.00000000000008527, -20.00000000000000000 ) ) ;
#11463 = CARTESIAN_POINT ( 'NONE',  ( 1.346194077712537629, 113.1875000000000284, 3.250000000000022649 ) ) ;
#11464 = CARTESIAN_POINT ( 'NONE',  ( 72.14031151490459592, 14.87472239508221072, -20.56889282981015654 ) ) ;
#11465 = ORIENTED_EDGE ( 'NONE', *, *, #8493, .F. ) ;
#11466 = VECTOR ( 'NONE', #11278, 1000.000000000000114 ) ;
#11467 = DIRECTION ( 'NONE',  ( 0.4999999999999878431, -0.8660254037844455910, 0.000000000000000000 ) ) ;
#11468 = ADVANCED_FACE ( 'NONE', ( #8915 ), #10735, .T. ) ;
#11469 = CARTESIAN_POINT ( 'NONE',  ( 2.500000000000000000, 1.768423874527823791, 1.020999999999998353 ) ) ;
#11470 = ORIENTED_EDGE ( 'NONE', *, *, #5883, .T. ) ;
#11471 = DIRECTION ( 'NONE',  ( 0.000000000000000000, 0.000000000000000000, -1.000000000000000000 ) ) ;
#11472 = ADVANCED_FACE ( 'NONE', ( #11685 ), #1149, .T. ) ;
#11473 = VECTOR ( 'NONE', #1046, 1000.000000000000114 ) ;
#11474 = VERTEX_POINT ( 'NONE', #10678 ) ;
#11475 = CARTESIAN_POINT ( 'NONE',  ( 5.525725221640833240, 18.86666975080242992, 79.50000000000000000 ) ) ;
#11476 = CARTESIAN_POINT ( 'NONE',  ( 74.16198487095665826, 40.00000000000009237, 25.00000000000000000 ) ) ;
#11477 = ORIENTED_EDGE ( 'NONE', *, *, #2892, .T. ) ;
#11478 = VECTOR ( 'NONE', #10622, 1000.000000000000000 ) ;
#11479 = CARTESIAN_POINT ( 'NONE',  ( 9.940467135547230271, 36.71530431672421457, 80.00000000000000000 ) ) ;
#11480 = FACE_OUTER_BOUND ( 'NONE', #10255, .T. ) ;
#11481 = ORIENTED_EDGE ( 'NONE', *, *, #927, .F. ) ;
#11482 = PRODUCT_CONTEXT ( 'NONE', #10425, 'mechanical' ) ;
#11483 = CYLINDRICAL_SURFACE ( 'NONE', #2894, 5.000000000000000888 ) ;
#11484 = AXIS2_PLACEMENT_3D ( 'NONE', #916, #5591, #855 ) ;
#11485 = DIRECTION ( 'NONE',  ( -0.000000000000000000, -0.000000000000000000, -1.000000000000000000 ) ) ;
#11486 = EDGE_CURVE ( 'NONE', #343, #366, #2142, .T. ) ;
#11487 = VERTEX_POINT ( 'NONE', #1208 ) ;
#11488 = CARTESIAN_POINT ( 'NONE',  ( -1.121994411437820416, 113.9999999986343937, -2.708734124999999882 ) ) ;
#11489 = DIRECTION ( 'NONE',  ( 0.000000000000000000, -0.8660254037844400399, -0.4999999999999974465 ) ) ;
#11490 = VECTOR ( 'NONE', #10731, 1000.000000000000000 ) ;
#11491 = VERTEX_POINT ( 'NONE', #6006 ) ;
#11492 = DIRECTION ( 'NONE',  ( -0.000000000000000000, 0.000000000000000000, 1.000000000000000000 ) ) ;
#11493 = CARTESIAN_POINT ( 'NONE',  ( 0.000000000000000000, 65.00000000000000000, 0.000000000000000000 ) ) ;
#11494 = EDGE_LOOP ( 'NONE', ( #7426, #6107, #6084, #8868 ) ) ;
#11495 = DIRECTION ( 'NONE',  ( 0.000000000000000000, -1.000000000000000000, 0.000000000000000000 ) ) ;
#11496 = LINE ( 'NONE', #9539, #10859 ) ;
#11497 = ORIENTED_EDGE ( 'NONE', *, *, #901, .F. ) ;
#11498 = B_SPLINE_CURVE_WITH_KNOTS ( 'NONE', 3,
 ( #2531, #11949, #10708, #3530, #9182, #2339, #8253, #6147, #5919, #8189 ),
 .UNSPECIFIED., .F., .F.,
 ( 4, 2, 2, 2, 4 ),
 ( 2.797157557069881010E-17, 0.001173140257025626076, 0.002346280514051213555, 0.003519420771076801468, 0.004692561028102389814 ),
 .UNSPECIFIED. ) ;
#11499 = LINE ( 'NONE', #4887, #11064 ) ;
#11500 = CARTESIAN_POINT ( 'NONE',  ( 0.000000000000000000, 345.0000000000000568, 0.000000000000000000 ) ) ;
#11501 = CARTESIAN_POINT ( 'NONE',  ( 0.000000000000000000, 127.0000000000000000, -22.00000000000000355 ) ) ;
#11502 = CARTESIAN_POINT ( 'NONE',  ( -27.69110892066586160, 86.46107124639166841, -11.72680205493506733 ) ) ;
#11503 = CARTESIAN_POINT ( 'NONE',  ( -2.298097038856279362, 111.3750000000000000, 2.298097038856279806 ) ) ;
#11504 = CIRCLE ( 'NONE', #6711, 9.999999999999998224 ) ;
#11505 = EDGE_CURVE ( 'NONE', #2264, #6899, #9889, .T. ) ;
#11506 = CARTESIAN_POINT ( 'NONE',  ( 1.915364268218908705, 113.4374999986344079, -1.915364268218909594 ) ) ;
#11507 = ORIENTED_EDGE ( 'NONE', *, *, #775, .F. ) ;
#11508 = DIRECTION ( 'NONE',  ( -0.000000000000000000, -1.000000000000000000, -0.000000000000000000 ) ) ;
#11509 = DIRECTION ( 'NONE',  ( 0.000000000000000000, 1.000000000000000000, 0.000000000000000000 ) ) ;
#11510 = ORIENTED_EDGE ( 'NONE', *, *, #351, .F. ) ;
#11511 = CARTESIAN_POINT ( 'NONE',  ( 0.000000000000000000, 65.00000000000000000, 0.000000000000000000 ) ) ;
#11512 = CARTESIAN_POINT ( 'NONE',  ( -13.00000000000000178, 127.0000000000000000, -7.483314773547880883 ) ) ;
#11513 = CARTESIAN_POINT ( 'NONE',  ( -25.00000000000000000, 570.2996408614167194, -31.99999999999999289 ) ) ;
#11514 = DIRECTION ( 'NONE',  ( 0.000000000000000000, 1.000000000000000000, 0.000000000000000000 ) ) ;
#11515 = EDGE_CURVE ( 'NONE', #8618, #12186, #10162, .T. ) ;
#11516 = EDGE_CURVE ( 'NONE', #10639, #10214, #8043, .T. ) ;
#11517 = EDGE_LOOP ( 'NONE', ( #6589, #11344, #10338, #3337 ) ) ;
#11518 = ORIENTED_EDGE ( 'NONE', *, *, #2409, .F. ) ;
#11519 = VERTEX_POINT ( 'NONE', #8292 ) ;
#11520 = CARTESIAN_POINT ( 'NONE',  ( 76.01088325117923716, 44.35544204059989681, -22.47665947743606907 ) ) ;
#11521 = SURFACE_STYLE_USAGE ( .BOTH. , #4913 ) ;
#11522 = DIRECTION ( 'NONE',  ( 0.000000000000000000, 1.000000000000000000, 0.000000000000000000 ) ) ;
#11523 = DIRECTION ( 'NONE',  ( 0.000000000000000000, 1.000000000000000000, 0.000000000000000000 ) ) ;
#11524 = DIRECTION ( 'NONE',  ( 0.000000000000000000, 0.000000000000000000, 1.000000000000000000 ) ) ;
#11525 = CARTESIAN_POINT ( 'NONE',  ( 76.01396467472481788, 15.64174653768074919, -22.47201498426100486 ) ) ;
#11526 = ORIENTED_EDGE ( 'NONE', *, *, #4405, .F. ) ;
#11527 = LINE ( 'NONE', #7590, #9031 ) ;
#11528 = CARTESIAN_POINT ( 'NONE',  ( 89.80805993797383735, 275.0000000000000000, 71.82974571984303225 ) ) ;
#11529 = ORIENTED_EDGE ( 'NONE', *, *, #5488, .F. ) ;
#11530 = DIRECTION ( 'NONE',  ( 0.8660254037844331565, -0.5000000000000095479, 0.000000000000000000 ) ) ;
#11531 = PRODUCT_DEFINITION_FORMATION_WITH_SPECIFIED_SOURCE ( 'ANY', '', #8455, .NOT_KNOWN. ) ;
#11532 = EDGE_CURVE ( 'NONE', #5901, #2816, #2566, .T. ) ;
#11533 = ORIENTED_EDGE ( 'NONE', *, *, #4563, .T. ) ;
#11534 = EDGE_CURVE ( 'NONE', #10229, #12186, #446, .T. ) ;
#11535 = DIRECTION ( 'NONE',  ( 1.000000000000000000, -0.000000000000000000, 1.224646799147353207E-16 ) ) ;
#11536 = LINE ( 'NONE', #297, #45 ) ;
#11537 = VERTEX_POINT ( 'NONE', #8166 ) ;
#11538 = LINE ( 'NONE', #10402, #6469 ) ;
#11539 = CARTESIAN_POINT ( 'NONE',  ( 0.000000000000000000, -5.000000000000000000, 0.000000000000000000 ) ) ;
#11540 = ORIENTED_EDGE ( 'NONE', *, *, #9498, .T. ) ;
#11541 = EDGE_CURVE ( 'NONE', #11491, #3929, #12347, .T. ) ;
#11542 = SHAPE_DEFINITION_REPRESENTATION ( #9553, #3316 ) ;
#11543 = AXIS2_PLACEMENT_3D ( 'NONE', #8747, #9869, #11823 ) ;
#11544 = CARTESIAN_POINT ( 'NONE',  ( 8.809218870694669690, 29.75000000000019540, 79.50000000000000000 ) ) ;
#11545 = FACE_OUTER_BOUND ( 'NONE', #6722, .T. ) ;
#11546 = ORIENTED_EDGE ( 'NONE', *, *, #8600, .F. ) ;
#11547 = CARTESIAN_POINT ( 'NONE',  ( 2.708734124999999882, 114.2499999986344079, -1.121994411437820638 ) ) ;
#11548 = CARTESIAN_POINT ( 'NONE',  ( -2.298097038856279362, 112.2499999972688158, 2.298097038856279806 ) ) ;
#11549 = VECTOR ( 'NONE', #5851, 1000.000000000000000 ) ;
#11550 = ORIENTED_EDGE ( 'NONE', *, *, #5332, .F. ) ;
#11551 = CARTESIAN_POINT ( 'NONE',  ( 5.092712519748611832, 18.61666975080242992, 80.00000000000000000 ) ) ;
#11552 = CARTESIAN_POINT ( 'NONE',  ( -14.00256363894252054, 22.13168096903907056, 73.68374432077325764 ) ) ;
#11553 = ORIENTED_EDGE ( 'NONE', *, *, #7340, .F. ) ;
#11554 = DIRECTION ( 'NONE',  ( 0.000000000000000000, 1.000000000000000000, 0.000000000000000000 ) ) ;
#11555 = DIRECTION ( 'NONE',  ( 0.000000000000000000, 0.000000000000000000, -1.000000000000000000 ) ) ;
#11556 = ORIENTED_EDGE ( 'NONE', *, *, #6439, .T. ) ;
#11557 = CARTESIAN_POINT ( 'NONE',  ( -5.970153145843347347E-16, 110.7500000000000000, -3.250000000000000444 ) ) ;
#11558 = LINE ( 'NONE', #5886, #337 ) ;
#11559 = LINE ( 'NONE', #6938, #2795 ) ;
#11560 = VECTOR ( 'NONE', #3794, 1000.000000000000000 ) ;
#11561 = CARTESIAN_POINT ( 'NONE',  ( -27.30107202361637775, 86.87046582918780757, -12.43589427268144831 ) ) ;
#11562 = CARTESIAN_POINT ( 'NONE',  ( 5.092712519748452848, 41.38333024919784719, 80.00000000000000000 ) ) ;
#11563 = CARTESIAN_POINT ( 'NONE',  ( -2.708734124999999882, 113.0624999986344079, 3.317242575922456639E-16 ) ) ;
#11564 = ORIENTED_EDGE ( 'NONE', *, *, #6041, .T. ) ;
#11565 = AXIS2_PLACEMENT_3D ( 'NONE', #7777, #4788, #8706 ) ;
#11566 = CIRCLE ( 'NONE', #814, 5.000000000000000888 ) ;
#11567 = CARTESIAN_POINT ( 'NONE',  ( 0.000000000000000000, 52.00000000000000711, 0.000000000000000000 ) ) ;
#11568 = DIRECTION ( 'NONE',  ( 0.000000000000000000, 1.000000000000000000, 0.000000000000000000 ) ) ;
#11569 = ORIENTED_EDGE ( 'NONE', *, *, #8475, .F. ) ;
#11570 = ADVANCED_FACE ( 'NONE', ( #4369 ), #8230, .F. ) ;
#11571 = CARTESIAN_POINT ( 'NONE',  ( 1.734723475976807094E-14, 65.00000000000000000, 57.08203932499370836 ) ) ;
#11572 = CARTESIAN_POINT ( 'NONE',  ( 0.000000000000000000, 87.50000000000000000, 0.000000000000000000 ) ) ;
#11573 = EDGE_CURVE ( 'NONE', #12241, #1921, #11745, .T. ) ;
#11574 = CARTESIAN_POINT ( 'NONE',  ( -34.84121487603211875, 75.26794919243111792, 7.660254037844449471 ) ) ;
#11575 = FACE_OUTER_BOUND ( 'NONE', #6650, .T. ) ;
#11576 = VECTOR ( 'NONE', #6896, 1000.000000000000114 ) ;
#11577 = AXIS2_PLACEMENT_3D ( 'NONE', #11112, #6374, #1638 ) ;
#11578 = B_SPLINE_CURVE_WITH_KNOTS ( 'NONE', 3,
 ( #6844, #9574, #2980, #4852 ),
 .UNSPECIFIED., .F., .F.,
 ( 4, 4 ),
 ( 0.000000000000000000, 0.002001274951694169586 ),
 .UNSPECIFIED. ) ;
#11579 = ORIENTED_EDGE ( 'NONE', *, *, #3947, .F. ) ;
#11580 = ORIENTED_EDGE ( 'NONE', *, *, #3103, .T. ) ;
#11581 = AXIS2_PLACEMENT_3D ( 'NONE', #8847, #1322, #5817 ) ;
#11582 = EDGE_CURVE ( 'NONE', #4135, #3932, #3180, .T. ) ;
#11583 = AXIS2_PLACEMENT_3D ( 'NONE', #8102, #3319, #4432 ) ;
#11584 = EDGE_CURVE ( 'NONE', #2607, #11110, #4371, .T. ) ;
#11585 = CARTESIAN_POINT ( 'NONE',  ( 69.85388127645428824, 17.99999999999971223, 31.17691453623957543 ) ) ;
#11586 = DIRECTION ( 'NONE',  ( -0.000000000000000000, -1.000000000000000000, 0.000000000000000000 ) ) ;
#11587 = VERTEX_POINT ( 'NONE', #3508 ) ;
#11588 = CARTESIAN_POINT ( 'NONE',  ( 0.000000000000000000, 290.0000000000000568, 95.00000000000002842 ) ) ;
#11589 = CARTESIAN_POINT ( 'NONE',  ( 71.13616097333213872, 16.84684309240030231, -23.96252879557480497 ) ) ;
#11590 = ORIENTED_EDGE ( 'NONE', *, *, #1588, .F. ) ;
#11591 = CARTESIAN_POINT ( 'NONE',  ( -1.346194077712548287, 111.6875000000000000, -3.250000000000012434 ) ) ;
#11592 = DIRECTION ( 'NONE',  ( 0.000000000000000000, 0.000000000000000000, 1.000000000000000000 ) ) ;
#11593 = AXIS2_PLACEMENT_3D ( 'NONE', #4217, #3222, #6904 ) ;
#11594 = ORIENTED_EDGE ( 'NONE', *, *, #1080, .F. ) ;
#11595 = CARTESIAN_POINT ( 'NONE',  ( -3.250000000000000444, 113.3749999972688158, 3.980102097228898231E-16 ) ) ;
#11596 = AXIS2_PLACEMENT_3D ( 'NONE', #10133, #9258, #12149 ) ;
#11597 = ADVANCED_FACE ( 'NONE', ( #9095 ), #8104, .T. ) ;
#11598 = EDGE_CURVE ( 'NONE', #5565, #1577, #11957, .T. ) ;
#11599 = ORIENTED_EDGE ( 'NONE', *, *, #11541, .T. ) ;
#11600 = DIRECTION ( 'NONE',  ( 0.4999999999999985012, 0.8660254037844394848, 0.000000000000000000 ) ) ;
#11601 = DIRECTION ( 'NONE',  ( -1.000000000000000000, 0.000000000000000000, -0.000000000000000000 ) ) ;
#11602 = ORIENTED_EDGE ( 'NONE', *, *, #9744, .F. ) ;
#11603 = CARTESIAN_POINT ( 'NONE',  ( 32.86043907464384972, 76.99999999999998579, -8.246007242324683517 ) ) ;
#11604 = CARTESIAN_POINT ( 'NONE',  ( 0.000000000000000000, 50.00000000000000000, 0.000000000000000000 ) ) ;
#11605 = ORIENTED_EDGE ( 'NONE', *, *, #4742, .F. ) ;
#11606 = CIRCLE ( 'NONE', #2835, 30.00000000000000711 ) ;
#11607 = SHAPE_DEFINITION_REPRESENTATION ( #1114, #10952 ) ;
#11608 = CARTESIAN_POINT ( 'NONE',  ( 11.80921887069467324, 29.83333333331263049, 80.00000048127353125 ) ) ;
#11609 = LINE ( 'NONE', #7732, #1621 ) ;
#11610 = ORIENTED_EDGE ( 'NONE', *, *, #3073, .T. ) ;
#11611 = CARTESIAN_POINT ( 'NONE',  ( 150.0000000000010516, 15.00000000000008527, 22.92893218813452094 ) ) ;
#11612 = PRODUCT_DEFINITION ( 'UNKNOWN', '', #979, #11752 ) ;
#11613 = CARTESIAN_POINT ( 'NONE',  ( 3.250000000000000444, 111.9374999972688016, 1.346194077712559389 ) ) ;
#11614 = AXIS2_PLACEMENT_3D ( 'NONE', #395, #3332, #2269 ) ;
#11615 = ORIENTED_EDGE ( 'NONE', *, *, #12206, .F. ) ;
#11616 = DIRECTION ( 'NONE',  ( 1.000000000000000000, 0.000000000000000000, -1.224646799147353207E-16 ) ) ;
#11617 = DIRECTION ( 'NONE',  ( 0.000000000000000000, 1.000000000000000000, -0.000000000000000000 ) ) ;
#11618 = ORIENTED_EDGE ( 'NONE', *, *, #5216, .T. ) ;
#11619 = DIRECTION ( 'NONE',  ( 0.000000000000000000, 1.000000000000000000, 0.000000000000000000 ) ) ;
#11620 = CARTESIAN_POINT ( 'NONE',  ( 20.55500000000001748, 3.061616997868384127E-16, -2.500000000000000888 ) ) ;
#11621 = EDGE_LOOP ( 'NONE', ( #4562, #6288, #12154, #7856 ) ) ;
#11622 = CARTESIAN_POINT ( 'NONE',  ( 74.16198487095665826, 15.00000000000008882, 25.00000000000000000 ) ) ;
#11623 = CARTESIAN_POINT ( 'NONE',  ( 0.000000000000000000, -10.00000000000000000, 70.00000000000001421 ) ) ;
#11624 = FACE_OUTER_BOUND ( 'NONE', #11827, .T. ) ;
#11625 = AXIS2_PLACEMENT_3D ( 'NONE', #10709, #11660, #1001 ) ;
#11626 = CARTESIAN_POINT ( 'NONE',  ( 21.00000000000000355, 0.000000000000000000, 0.000000000000000000 ) ) ;
#11627 = DIRECTION ( 'NONE',  ( 0.000000000000000000, 0.000000000000000000, -1.000000000000000000 ) ) ;
#11628 = EDGE_CURVE ( 'NONE', #1631, #5677, #3321, .T. ) ;
#11629 = CARTESIAN_POINT ( 'NONE',  ( 2.708734124999999882, 113.6249999986344079, 1.121994411437819084 ) ) ;
#11630 = ORIENTED_EDGE ( 'NONE', *, *, #8589, .F. ) ;
#11631 = VECTOR ( 'NONE', #1850, 1000.000000000000000 ) ;
#11632 = VERTEX_POINT ( 'NONE', #9917 ) ;
#11633 = CARTESIAN_POINT ( 'NONE',  ( 145.0000000000011369, 65.00000000000000000, 25.00000000000000000 ) ) ;
#11634 = CARTESIAN_POINT ( 'NONE',  ( -1.190781129305471087, 30.00000000000008882, 80.00000000000000000 ) ) ;
#11635 = ORIENTED_EDGE ( 'NONE', *, *, #9007, .F. ) ;
#11636 = CARTESIAN_POINT ( 'NONE',  ( -12.32411137850302119, 23.28349364905396612, 79.50000000000000000 ) ) ;
#11637 = DIRECTION ( 'NONE',  ( 1.000000000000000000, 0.000000000000000000, 0.000000000000000000 ) ) ;
#11638 = LINE ( 'NONE', #11513, #11687 ) ;
#11639 = CARTESIAN_POINT ( 'NONE',  ( -27.96741528345882344, 86.27927944434871677, -11.41192941739715927 ) ) ;
#11640 = CIRCLE ( 'NONE', #278, 15.00000000000000000 ) ;
#11641 = ORIENTED_EDGE ( 'NONE', *, *, #1804, .F. ) ;
#11642 = ADVANCED_FACE ( 'NONE', ( #7121 ), #8400, .F. ) ;
#11643 = EDGE_CURVE ( 'NONE', #9081, #11877, #6339, .T. ) ;
#11644 = CARTESIAN_POINT ( 'NONE',  ( -7.907287480251421030, 41.13333024919781167, 79.50000000000000000 ) ) ;
#11645 = CARTESIAN_POINT ( 'NONE',  ( 0.000000000000000000, 110.0000000000000000, 0.000000000000000000 ) ) ;
#11646 = ORIENTED_EDGE ( 'NONE', *, *, #6398, .F. ) ;
#11647 = AXIS2_PLACEMENT_3D ( 'NONE', #4661, #3669, #11339 ) ;
#11648 = DIRECTION ( 'NONE',  ( 1.000000000000000000, 0.000000000000000000, 0.000000000000000000 ) ) ;
#11649 = CARTESIAN_POINT ( 'NONE',  ( 72.46134176498783575, 10.00000000076808249, -19.35843010035823397 ) ) ;
#11650 = CARTESIAN_POINT ( 'NONE',  ( 71.66575360104040726, 10.66092814062295346, -22.11578253505649272 ) ) ;
#11651 = DIRECTION ( 'NONE',  ( 0.000000000000000000, 0.000000000000000000, -1.000000000000000000 ) ) ;
#11652 = ORIENTED_EDGE ( 'NONE', *, *, #7271, .F. ) ;
#11653 = CARTESIAN_POINT ( 'NONE',  ( 6.000000000000000000, 62.00000000000000000, 70.00000000000001421 ) ) ;
#11654 = EDGE_CURVE ( 'NONE', #4316, #9884, #8722, .T. ) ;
#11655 = ADVANCED_FACE ( 'NONE', ( #4418 ), #3490, .T. ) ;
#11656 = CIRCLE ( 'NONE', #6272, 17.50000000000000000 ) ;
#11657 = AXIS2_PLACEMENT_3D ( 'NONE', #8175, #4315, #5203 ) ;
#11658 = ORIENTED_EDGE ( 'NONE', *, *, #1891, .F. ) ;
#11659 = CARTESIAN_POINT ( 'NONE',  ( -12.32202939415815912, 36.71530431672423589, 80.00000000000000000 ) ) ;
#11660 = DIRECTION ( 'NONE',  ( 0.000000000000000000, 1.000000000000000000, 0.000000000000000000 ) ) ;
#11661 = ORIENTED_EDGE ( 'NONE', *, *, #2689, .F. ) ;
#11662 = CARTESIAN_POINT ( 'NONE',  ( 1.347111479062088996E-14, 340.0000000000000000, -110.0000000000000284 ) ) ;
#11663 = FACE_OUTER_BOUND ( 'NONE', #3461, .T. ) ;
#11664 = ORIENTED_EDGE ( 'NONE', *, *, #11264, .F. ) ;
#11665 = CARTESIAN_POINT ( 'NONE',  ( 140.0000000000011369, 225.0000000000000853, 20.00000000000000000 ) ) ;
#11666 = DIRECTION ( 'NONE',  ( 0.000000000000000000, 1.000000000000000000, 0.000000000000000000 ) ) ;
#11667 = EDGE_CURVE ( 'NONE', #1995, #10879, #9141, .T. ) ;
#11668 = ORIENTED_EDGE ( 'NONE', *, *, #5843, .T. ) ;
#11669 = CARTESIAN_POINT ( 'NONE',  ( 2.708734124999999882, 112.2499999986344079, -1.121994411437820638 ) ) ;
#11670 = CARTESIAN_POINT ( 'NONE',  ( -3.250000000000001776, 114.4374999972688158, -1.346194077712558723 ) ) ;
#11671 = AXIS2_PLACEMENT_3D ( 'NONE', #8542, #5004, #3008 ) ;
#11672 = ADVANCED_BREP_SHAPE_REPRESENTATION ( '', ( #8720, #1612 ), #4147 ) ;
#11673 = EDGE_LOOP ( 'NONE', ( #6329, #3495, #9604 ) ) ;
#11674 = DIRECTION ( 'NONE',  ( 0.000000000000000000, 0.000000000000000000, 1.000000000000000000 ) ) ;
#11675 = FACE_OUTER_BOUND ( 'NONE', #6954, .T. ) ;
#11676 = EDGE_LOOP ( 'NONE', ( #1378, #9920, #1956 ) ) ;
#11677 = AXIS2_PLACEMENT_3D ( 'NONE', #1059, #4929, #7900 ) ;
#11678 = LINE ( 'NONE', #3190, #6394 ) ;
#11679 = CARTESIAN_POINT ( 'NONE',  ( -7.907287480251421030, 41.13333024919781167, 79.50000000000000000 ) ) ;
#11680 = VERTEX_POINT ( 'NONE', #10142 ) ;
#11681 = CARTESIAN_POINT ( 'NONE',  ( 0.000000000000000000, 265.0000000000000000, 0.000000000000000000 ) ) ;
#11682 = LINE ( 'NONE', #8040, #3924 ) ;
#11683 = LINE ( 'NONE', #4367, #6400 ) ;
#11684 = VERTEX_POINT ( 'NONE', #11029 ) ;
#11685 = FACE_OUTER_BOUND ( 'NONE', #11204, .T. ) ;
#11686 = CARTESIAN_POINT ( 'NONE',  ( -1.915364268218909594, 114.1874999986344079, -1.915364268218908927 ) ) ;
#11687 = VECTOR ( 'NONE', #11451, 1000.000000000000000 ) ;
#11688 = ORIENTED_EDGE ( 'NONE', *, *, #6169, .F. ) ;
#11689 = ORIENTED_EDGE ( 'NONE', *, *, #6942, .F. ) ;
#11690 = EDGE_CURVE ( 'NONE', #7113, #7236, #807, .T. ) ;
#11691 = CARTESIAN_POINT ( 'NONE',  ( 0.000000000000000000, 67.00000000000000000, 0.000000000000000000 ) ) ;
#11692 = EDGE_CURVE ( 'NONE', #3272, #9269, #6965, .T. ) ;
#11693 = DIRECTION ( 'NONE',  ( 0.000000000000000000, 1.000000000000000000, 0.000000000000000000 ) ) ;
#11694 = EDGE_LOOP ( 'NONE', ( #7901, #12070 ) ) ;
#11695 = DIRECTION ( 'NONE',  ( -0.000000000000000000, 1.000000000000000000, -0.000000000000000000 ) ) ;
#11696 = DIRECTION ( 'NONE',  ( 1.000000000000000000, 0.000000000000000000, 0.000000000000000000 ) ) ;
#11697 = AXIS2_PLACEMENT_3D ( 'NONE', #3824, #11372, #9606 ) ;
#11698 = DIRECTION ( 'NONE',  ( 0.000000000000000000, 0.000000000000000000, 1.000000000000000000 ) ) ;
#11699 = LINE ( 'NONE', #10752, #7778 ) ;
#11700 = EDGE_CURVE ( 'NONE', #1669, #7450, #1592, .T. ) ;
#11701 =( NAMED_UNIT ( * ) SI_UNIT ( $, .STERADIAN. ) SOLID_ANGLE_UNIT ( ) );
#11702 = ORIENTED_EDGE ( 'NONE', *, *, #7673, .T. ) ;
#11703 = SURFACE_STYLE_FILL_AREA ( #2103 ) ;
#11704 = CARTESIAN_POINT ( 'NONE',  ( -116.4243635975518742, 285.0000000000000568, 45.50129185973785440 ) ) ;
#11705 = CARTESIAN_POINT ( 'NONE',  ( 0.000000000000000000, 0.000000000000000000, 79.50000000000000000 ) ) ;
#11706 = FILL_AREA_STYLE_COLOUR ( '', #8059 ) ;
#11707 = CARTESIAN_POINT ( 'NONE',  ( 70.67711243716091474, 12.63198440090825869, -25.09579365358156622 ) ) ;
#11708 = CARTESIAN_POINT ( 'NONE',  ( 0.000000000000000000, 110.0000000000000000, 3.250000000000000444 ) ) ;
#11709 = CARTESIAN_POINT ( 'NONE',  ( -4.975863863883684959E-16, 112.0624999986344079, -2.708734125000000326 ) ) ;
#11710 =( REPRESENTATION_RELATIONSHIP ('NONE','NONE', #3713, #7136 ) REPRESENTATION_RELATIONSHIP_WITH_TRANSFORMATION ( #1996 )SHAPE_REPRESENTATION_RELATIONSHIP( ) );
#11711 = EDGE_LOOP ( 'NONE', ( #11668, #12238, #3172 ) ) ;
#11712 = CARTESIAN_POINT ( 'NONE',  ( 7.594472908538985045, 34.78349364905407270, 80.00000000000000000 ) ) ;
#11713 = CIRCLE ( 'NONE', #7720, 0.5000000000000004441 ) ;
#11714 = VERTEX_POINT ( 'NONE', #2492 ) ;
#11715 = CARTESIAN_POINT ( 'NONE',  ( 2.500000000000000000, -1.768423874527823569, 1.021000000000002350 ) ) ;
#11716 = ORIENTED_EDGE ( 'NONE', *, *, #10287, .F. ) ;
#11717 = DIRECTION ( 'NONE',  ( 0.000000000000000000, 1.000000000000000000, 0.000000000000000000 ) ) ;
#11718 = LINE ( 'NONE', #1307, #4697 ) ;
#11719 = ORIENTED_EDGE ( 'NONE', *, *, #713, .T. ) ;
#11720 = EDGE_CURVE ( 'NONE', #2552, #12150, #11443, .T. ) ;
#11721 = CARTESIAN_POINT ( 'NONE',  ( 7.344472908539098732, 24.78349364905406205, 79.50000000000000000 ) ) ;
#11722 = DIRECTION ( 'NONE',  ( -1.000000000000000000, -0.000000000000000000, -0.000000000000000000 ) ) ;
#11723 = AXIS2_PLACEMENT_3D ( 'NONE', #2647, #8313, #2767 ) ;
#11724 = PRODUCT_DEFINITION_FORMATION_WITH_SPECIFIED_SOURCE ( 'ANY', '', #207, .NOT_KNOWN. ) ;
#11725 = ORIENTED_EDGE ( 'NONE', *, *, #3275, .F. ) ;
#11726 = CARTESIAN_POINT ( 'NONE',  ( 1.915364268218909594, 113.4374999986344079, 1.915364268218909594 ) ) ;
#11727 = ORIENTED_EDGE ( 'NONE', *, *, #7837, .T. ) ;
#11728 = EDGE_CURVE ( 'NONE', #11037, #6417, #8902, .T. ) ;
#11729 = DIRECTION ( 'NONE',  ( 0.000000000000000000, 1.000000000000000000, 0.000000000000000000 ) ) ;
#11730 = LINE ( 'NONE', #5068, #7469 ) ;
#11731 = EDGE_CURVE ( 'NONE', #3140, #5735, #367, .T. ) ;
#11732 = ORIENTED_EDGE ( 'NONE', *, *, #215, .T. ) ;
#11733 = CARTESIAN_POINT ( 'NONE',  ( -75.98513253586240523, 285.0000000000000568, 72.46557550663233371 ) ) ;
#11734 = CARTESIAN_POINT ( 'NONE',  ( 3.092233167847066435E-15, 87.50000000000000000, -24.99999999999999645 ) ) ;
#11735 = ORIENTED_EDGE ( 'NONE', *, *, #6920, .T. ) ;
#11736 = DIRECTION ( 'NONE',  ( 0.000000000000000000, 0.000000000000000000, 1.000000000000000000 ) ) ;
#11737 = DIRECTION ( 'NONE',  ( 0.000000000000000000, 1.000000000000000000, 0.000000000000000000 ) ) ;
#11738 = CARTESIAN_POINT ( 'NONE',  ( 0.000000000000000000, 67.00000000000000000, 0.000000000000000000 ) ) ;
#11739 = ORIENTED_EDGE ( 'NONE', *, *, #3541, .T. ) ;
#11740 = LINE ( 'NONE', #4131, #8353 ) ;
#11741 = CARTESIAN_POINT ( 'NONE',  ( 69.72804008650275875, 16.70676746007779911, 27.62368211345550506 ) ) ;
#11742 = AXIS2_PLACEMENT_3D ( 'NONE', #2551, #6597, #10393 ) ;
#11743 = AXIS2_PLACEMENT_3D ( 'NONE', #5995, #11729, #2244 ) ;
#11744 = COLOUR_RGB ( '', 0.08235294, 0.09019608, 0.10196078) ;
#11745 =( BOUNDED_CURVE ( )  B_SPLINE_CURVE ( 2, ( #1575, #9035, #637, #7183, #6251, #5377, #509, #5317, #7312 ),
 .UNSPECIFIED., .F., .T. ) 
 B_SPLINE_CURVE_WITH_KNOTS ( ( 3, 2, 2, 2, 3 ),
 ( 0.4375000000000003886, 0.4687500000000003886, 0.5000000000000004441, 0.5312500000000004441, 0.5625000000000004441 ),
 .UNSPECIFIED. ) 
 CURVE ( )  GEOMETRIC_REPRESENTATION_ITEM ( )  RATIONAL_B_SPLINE_CURVE ( ( 0.9999999999999990008, 0.9238795325112877377, 1.000000000000000000, 0.9238795325112867385, 1.000000000000000000, 0.9238795325112867385, 1.000000000000000000, 0.9238795325112856283, 1.000000000000001110 ) ) 
 REPRESENTATION_ITEM ( '' )  );
#11746 = EDGE_CURVE ( 'NONE', #9474, #10742, #12140, .T. ) ;
#11747 = ORIENTED_EDGE ( 'NONE', *, *, #7040, .T. ) ;
#11748 = ADVANCED_FACE ( 'NONE', ( #7231 ), #5551, .T. ) ;
#11749 = PLANE ( 'NONE',  #1102 ) ;
#11750 = CARTESIAN_POINT ( 'NONE',  ( 74.37657609242708645, 41.64661626995485477, -24.73263046052358405 ) ) ;
#11751 = VERTEX_POINT ( 'NONE', #9328 ) ;
#11752 = PRODUCT_DEFINITION_CONTEXT ( 'detailed design', #3826, 'design' ) ;
#11753 = DIRECTION ( 'NONE',  ( -0.000000000000000000, 0.000000000000000000, -1.000000000000000000 ) ) ;
#11754 = CARTESIAN_POINT ( 'NONE',  ( 76.47662455941971871, 44.68978179728624411, 21.74119912861985071 ) ) ;
#11755 = ORIENTED_EDGE ( 'NONE', *, *, #10125, .F. ) ;
#11756 = FACE_OUTER_BOUND ( 'NONE', #7892, .T. ) ;
#11757 = AXIS2_PLACEMENT_3D ( 'NONE', #10795, #10552, #9854 ) ;
#11758 = CARTESIAN_POINT ( 'NONE',  ( -14.19078112930533209, 29.75000000000008882, 79.50000000000000000 ) ) ;
#11759 = LINE ( 'NONE', #399, #531 ) ;
#11760 = CARTESIAN_POINT ( 'NONE',  ( 1.658621287961228566E-16, 110.5624999986344079, 2.708734125000000326 ) ) ;
#11761 = VERTEX_POINT ( 'NONE', #7479 ) ;
#11762 = APPLICATION_PROTOCOL_DEFINITION ( 'draft international standard', 'automotive_design', 1998, #641 ) ;
#11763 = EDGE_CURVE ( 'NONE', #1199, #6472, #8152, .T. ) ;
#11764 = ORIENTED_EDGE ( 'NONE', *, *, #9281, .F. ) ;
#11765 = EDGE_CURVE ( 'NONE', #10685, #4433, #3550, .T. ) ;
#11766 = AXIS2_PLACEMENT_3D ( 'NONE', #6221, #607, #6967 ) ;
#11767 = EDGE_CURVE ( 'NONE', #5388, #10667, #11348, .T. ) ;
#11768 = DIRECTION ( 'NONE',  ( 0.000000000000000000, 0.000000000000000000, -1.000000000000000000 ) ) ;
#11769 = CARTESIAN_POINT ( 'NONE',  ( 77.45966692414835109, 10.00000000000008882, -19.99999999999999645 ) ) ;
#11770 =( BOUNDED_CURVE ( )  B_SPLINE_CURVE ( 2, ( #3297, #4412, #8205, #11091, #6162, #9956, #489, #2546, #11787 ),
 .UNSPECIFIED., .F., .F. ) 
 B_SPLINE_CURVE_WITH_KNOTS ( ( 3, 2, 2, 2, 3 ),
 ( 0.6875000000000005551, 0.7187500000000005551, 0.7500000000000006661, 0.7812500000000006661, 0.8125000000000006661 ),
 .UNSPECIFIED. ) 
 CURVE ( )  GEOMETRIC_REPRESENTATION_ITEM ( )  RATIONAL_B_SPLINE_CURVE ( ( 0.9999999999999986677, 0.9238795325112880708, 1.000000000000000000, 0.9238795325112867385, 1.000000000000000000, 0.9238795325112867385, 1.000000000000000000, 0.9238795325112850731, 1.000000000000001554 ) ) 
 REPRESENTATION_ITEM ( '' )  );
#11771 = CARTESIAN_POINT ( 'NONE',  ( 30.00000000000004263, 65.00000000000000000, -63.24555320336758513 ) ) ;
#11772 = SURFACE_STYLE_USAGE ( .BOTH. , #8757 ) ;
#11773 = VECTOR ( 'NONE', #1205, 1000.000000000000000 ) ;
#11774 = CARTESIAN_POINT ( 'NONE',  ( 0.000000000000000000, 122.5000000000000000, 17.00000000000000000 ) ) ;
#11775 = PRESENTATION_LAYER_ASSIGNMENT (  '', '', ( #10160 ) ) ;
#11776 = CARTESIAN_POINT ( 'NONE',  ( 0.000000000000000000, 10.00000000000017586, 0.000000000000000000 ) ) ;
#11777 = PRODUCT ( 'BR-821', 'BR-821', '', ( #7753 ) ) ;
#11778 = CARTESIAN_POINT ( 'NONE',  ( 2.298097038856279806, 110.1250000000000000, 2.298097038856279806 ) ) ;
#11779 = ORIENTED_EDGE ( 'NONE', *, *, #9142, .T. ) ;
#11780 = FACE_OUTER_BOUND ( 'NONE', #11406, .T. ) ;
#11781 = EDGE_CURVE ( 'NONE', #10546, #9044, #4725, .T. ) ;
#11782 = CIRCLE ( 'NONE', #10771, 100.0000000000000284 ) ;
#11783 = ORIENTED_EDGE ( 'NONE', *, *, #5415, .T. ) ;
#11784 = DIRECTION ( 'NONE',  ( 0.000000000000000000, 0.4999999999999976685, 0.8660254037844399289 ) ) ;
#11785 = EDGE_LOOP ( 'NONE', ( #9018, #5863, #7360, #3975 ) ) ;
#11786 = DIRECTION ( 'NONE',  ( 0.000000000000000000, 1.000000000000000000, 0.000000000000000000 ) ) ;
#11787 = CARTESIAN_POINT ( 'NONE',  ( 1.990051048614449116E-16, 114.1249999972688158, 3.250000000000000444 ) ) ;
#11788 = ORIENTED_EDGE ( 'NONE', *, *, #1021, .T. ) ;
#11789 = CIRCLE ( 'NONE', #5015, 10.00000000000000178 ) ;
#11790 = FACE_OUTER_BOUND ( 'NONE', #811, .T. ) ;
#11791 = CIRCLE ( 'NONE', #6409, 17.00000000000000000 ) ;
#11792 = CARTESIAN_POINT ( 'NONE',  ( -31.00813199677072163, 87.06416249055504863, -8.771386731425975469 ) ) ;
#11793 = CONTEXT_DEPENDENT_SHAPE_REPRESENTATION ( #6376, #8865 ) ;
#11794 = ORIENTED_EDGE ( 'NONE', *, *, #11746, .T. ) ;
#11795 = CARTESIAN_POINT ( 'NONE',  ( 69.53296405455485285, 40.65417715541234855, -28.10992626845828113 ) ) ;
#11796 = EDGE_CURVE ( 'NONE', #2993, #6640, #9136, .T. ) ;
#11797 = EDGE_CURVE ( 'NONE', #4222, #8405, #3611, .T. ) ;
#11798 = VERTEX_POINT ( 'NONE', #12100 ) ;
#11799 = CARTESIAN_POINT ( 'NONE',  ( 31.92482683647866892, 87.00000000000011369, 8.660254037844589803 ) ) ;
#11800 = PLANE ( 'NONE',  #11407 ) ;
#11801 = ORIENTED_EDGE ( 'NONE', *, *, #770, .F. ) ;
#11802 = DIRECTION ( 'NONE',  ( 0.000000000000000000, 0.000000000000000000, 1.000000000000000000 ) ) ;
#11803 = CARTESIAN_POINT ( 'NONE',  ( 70.88282142915605277, 12.08604768574887345, 24.51348554696365056 ) ) ;
#11804 = EDGE_LOOP ( 'NONE', ( #11991, #7987, #9895, #958, #7999, #11000, #2782 ) ) ;
#11805 = CARTESIAN_POINT ( 'NONE',  ( -100.7495955565347288, 275.0000000000000000, 29.57226733266632124 ) ) ;
#11806 = CARTESIAN_POINT ( 'NONE',  ( 76.23711339313383917, 44.53569103644999672, -22.12715364262389528 ) ) ;
#11807 = PLANE ( 'NONE',  #8569 ) ;
#11808 = ORIENTED_EDGE ( 'NONE', *, *, #9794, .T. ) ;
#11809 = DIRECTION ( 'NONE',  ( -0.000000000000000000, 1.000000000000000000, -0.000000000000000000 ) ) ;
#11810 = CIRCLE ( 'NONE', #9999, 70.00000000000001421 ) ;
#11811 = CARTESIAN_POINT ( 'NONE',  ( 72.28000013808933488, 14.83797322639769689, 20.04822706562307033 ) ) ;
#11812 = EDGE_CURVE ( 'NONE', #8980, #11984, #10748, .T. ) ;
#11813 = VERTEX_POINT ( 'NONE', #6482 ) ;
#11814 = CARTESIAN_POINT ( 'NONE',  ( 72.45961080413241007, 49.99999999876575885, -19.36513408292425709 ) ) ;
#11815 = LINE ( 'NONE', #3258, #1882 ) ;
#11816 = ORIENTED_EDGE ( 'NONE', *, *, #11440, .F. ) ;
#11817 = EDGE_CURVE ( 'NONE', #10746, #7164, #4541, .T. ) ;
#11818 = CARTESIAN_POINT ( 'NONE',  ( 11.80921887069467324, 30.25000000000018474, 80.00000000000000000 ) ) ;
#11819 = CARTESIAN_POINT ( 'NONE',  ( 70.86094439463602157, 41.47042339171561309, 24.79386831723889628 ) ) ;
#11820 = AXIS2_PLACEMENT_3D ( 'NONE', #5431, #6546, #6489 ) ;
#11821 = ORIENTED_EDGE ( 'NONE', *, *, #8297, .T. ) ;
#11822 = LINE ( 'NONE', #8927, #5236 ) ;
#11823 = DIRECTION ( 'NONE',  ( 0.000000000000000000, 0.000000000000000000, 1.000000000000000000 ) ) ;
#11824 = DIRECTION ( 'NONE',  ( 0.8660254037844331565, -0.5000000000000095479, 0.000000000000000000 ) ) ;
#11825 = CARTESIAN_POINT ( 'NONE',  ( -2.708734125000000326, 111.7499999986343795, 1.121994411437819084 ) ) ;
#11826 = EDGE_CURVE ( 'NONE', #1374, #6508, #12155, .T. ) ;
#11827 = EDGE_LOOP ( 'NONE', ( #5608, #9950, #4946, #5418 ) ) ;
#11828 = AXIS2_PLACEMENT_3D ( 'NONE', #9504, #2104, #8631 ) ;
#11829 = CARTESIAN_POINT ( 'NONE',  ( 10.06754911989233392, 36.50000000000012079, 80.00000000000000000 ) ) ;
#11830 = DIRECTION ( 'NONE',  ( -1.000000000000000000, 0.000000000000000000, 0.000000000000000000 ) ) ;
#11831 = DIRECTION ( 'NONE',  ( -0.000000000000000000, 1.000000000000000000, -0.000000000000000000 ) ) ;
#11832 = CARTESIAN_POINT ( 'NONE',  ( 32.32195836398363298, 75.59155356138302295, -7.099754829268524858 ) ) ;
#11833 = ITEM_DEFINED_TRANSFORMATION ( 'NONE', 'NONE', #9111,  #1612 ) ;
#11834 = PRODUCT_DEFINITION ( 'UNKNOWN', '', #5351, #2265 ) ;
#11835 = VECTOR ( 'NONE', #9180, 1000.000000000000000 ) ;
#11836 = AXIS2_PLACEMENT_3D ( 'NONE', #8224, #8288, #4430 ) ;
#11837 = DIRECTION ( 'NONE',  ( -0.000000000000000000, 1.000000000000000000, -0.000000000000000000 ) ) ;
#11838 = CARTESIAN_POINT ( 'NONE',  ( 1.915364268218908927, 111.1874999986344079, -1.915364268218909816 ) ) ;
#11839 = ORIENTED_EDGE ( 'NONE', *, *, #5598, .F. ) ;
#11840 = DIRECTION ( 'NONE',  ( -0.000000000000000000, -1.000000000000000000, 0.000000000000000000 ) ) ;
#11841 = CIRCLE ( 'NONE', #2275, 4.000000000000000000 ) ;
#11842 = SHAPE_REPRESENTATION ( 'Stainless Steel S-Blade Unit', ( #1612 ), #10102 ) ;
#11843 = VECTOR ( 'NONE', #6908, 1000.000000000000000 ) ;
#11844 = VERTEX_POINT ( 'NONE', #8518 ) ;
#11845 = CARTESIAN_POINT ( 'NONE',  ( 0.000000000000000000, 127.0000000000000000, 0.000000000000000000 ) ) ;
#11846 = VERTEX_POINT ( 'NONE', #12342 ) ;
#11847 = CARTESIAN_POINT ( 'NONE',  ( 0.000000000000000000, 285.0000000000000568, 0.000000000000000000 ) ) ;
#11848 = EDGE_CURVE ( 'NONE', #2576, #2418, #8399, .T. ) ;
#11849 = CARTESIAN_POINT ( 'NONE',  ( 77.45966692414835109, 15.00000000000008882, -19.99999999999999645 ) ) ;
#11850 = ORIENTED_EDGE ( 'NONE', *, *, #10766, .T. ) ;
#11851 = CARTESIAN_POINT ( 'NONE',  ( -5.970153145843347347E-16, 110.7500000000000000, -3.250000000000000444 ) ) ;
#11852 = CARTESIAN_POINT ( 'NONE',  ( 25.00000000000000000, 345.0000000000000568, -90.00000000000000000 ) ) ;
#11853 = ADVANCED_FACE ( 'NONE', ( #1680 ), #9453, .T. ) ;
#11854 = VECTOR ( 'NONE', #10527, 1000.000000000000000 ) ;
#11855 = ORIENTED_EDGE ( 'NONE', *, *, #2888, .F. ) ;
#11856 = DIRECTION ( 'NONE',  ( 1.000000000000000000, -0.000000000000000000, 0.000000000000000000 ) ) ;
#11857 = CIRCLE ( 'NONE', #6664, 14.99999999999999822 ) ;
#11858 = ORIENTED_EDGE ( 'NONE', *, *, #9434, .T. ) ;
#11859 = CARTESIAN_POINT ( 'NONE',  ( 3.122849337825750222E-15, 92.00000000000000000, 25.50000000000000000 ) ) ;
#11860 = CARTESIAN_POINT ( 'NONE',  ( -3.250000000000001776, 114.4374999972688158, -1.346194077712558279 ) ) ;
#11861 = ORIENTED_EDGE ( 'NONE', *, *, #10287, .T. ) ;
#11862 = TOROIDAL_SURFACE ( 'NONE', #2263, 105.0000000000000284, 5.000000000000000000 ) ;
#11863 = CYLINDRICAL_SURFACE ( 'NONE', #10372, 5.000000000000004441 ) ;
#11864 = DIRECTION ( 'NONE',  ( -0.000000000000000000, -1.000000000000000000, 0.000000000000000000 ) ) ;
#11865 = EDGE_LOOP ( 'NONE', ( #9351, #203, #2836, #4472 ) ) ;
#11866 = PLANE ( 'NONE',  #8029 ) ;
#11867 = CARTESIAN_POINT ( 'NONE',  ( 0.000000000000000000, 67.00000000000000000, -72.00000000000002842 ) ) ;
#11868 = DIRECTION ( 'NONE',  ( 0.000000000000000000, 0.000000000000000000, 1.000000000000000000 ) ) ;
#11869 = VERTEX_POINT ( 'NONE', #11289 ) ;
#11870 = CARTESIAN_POINT ( 'NONE',  ( 27.67899820261485999, 88.38261385519929547, 11.05501148229834030 ) ) ;
#11871 = CARTESIAN_POINT ( 'NONE',  ( 71.78384618016828256, 10.51296179634712580, 21.72949947218171118 ) ) ;
#11872 = AXIS2_PLACEMENT_3D ( 'NONE', #4067, #10670, #6812 ) ;
#11873 = AXIS2_PLACEMENT_3D ( 'NONE', #10517, #9757, #6718 ) ;
#11874 = EDGE_LOOP ( 'NONE', ( #11259, #4740, #5768, #5072 ) ) ;
#11875 = FACE_OUTER_BOUND ( 'NONE', #2831, .T. ) ;
#11876 = CARTESIAN_POINT ( 'NONE',  ( -25.00000000000000000, 570.2996408614167194, -88.00000000000000000 ) ) ;
#11877 = VERTEX_POINT ( 'NONE', #3672 ) ;
#11878 = CYLINDRICAL_SURFACE ( 'NONE', #9824, 5.000000000000000888 ) ;
#11879 = CARTESIAN_POINT ( 'NONE',  ( 71.31012073601122836, 43.75331323920969595, 23.41524959671097150 ) ) ;
#11880 = EDGE_LOOP ( 'NONE', ( #3444, #9611, #9845, #11023 ) ) ;
#11881 = CARTESIAN_POINT ( 'NONE',  ( 2.500000000000000000, 2.357898499370431722, -2.818925648462311528E-15 ) ) ;
#11882 = DIRECTION ( 'NONE',  ( 0.000000000000000000, 1.000000000000000000, 0.000000000000000000 ) ) ;
#11883 = CARTESIAN_POINT ( 'NONE',  ( 4.999999999999997335, 0.000000000000000000, 4.250000000000000000 ) ) ;
#11884 = CARTESIAN_POINT ( 'NONE',  ( -1.915364268218909150, 111.6874999986344079, 1.915364268218909594 ) ) ;
#11885 = EDGE_CURVE ( 'NONE', #4534, #8555, #396, .T. ) ;
#11886 = STYLED_ITEM ( 'NONE', ( #2332 ), #8859 ) ;
#11887 = ORIENTED_EDGE ( 'NONE', *, *, #2087, .T. ) ;
#11888 = UNCERTAINTY_MEASURE_WITH_UNIT (LENGTH_MEASURE( 1.000000000000000082E-05 ), #9501, 'distance_accuracy_value', 'NONE');
#11889 = TOROIDAL_SURFACE ( 'NONE', #6516, 25.00000000000000000, 10.00000000000000000 ) ;
#11890 = LINE ( 'NONE', #1656, #11835 ) ;
#11891 = CARTESIAN_POINT ( 'NONE',  ( -14.19078112930533031, 30.00000000000017764, 80.00000000000000000 ) ) ;
#11892 = ADVANCED_FACE ( 'NONE', ( #9391 ), #4664, .T. ) ;
#11893 = EDGE_CURVE ( 'NONE', #1518, #4574, #10550, .T. ) ;
#11894 = DIRECTION ( 'NONE',  ( 0.000000000000000000, 0.000000000000000000, -1.000000000000000000 ) ) ;
#11895 = CYLINDRICAL_SURFACE ( 'NONE', #11188, 3.399999999999999911 ) ;
#11896 =( BOUNDED_CURVE ( )  B_SPLINE_CURVE ( 2, ( #7502, #1826, #1948, #12305, #9538 ),
 .UNSPECIFIED., .F., .F. ) 
 B_SPLINE_CURVE_WITH_KNOTS ( ( 3, 2, 3 ),
 ( 0.000000000000000000, 0.03125000000000002776, 0.06250000000000005551 ),
 .UNSPECIFIED. ) 
 CURVE ( )  GEOMETRIC_REPRESENTATION_ITEM ( )  RATIONAL_B_SPLINE_CURVE ( ( 1.000000000000000000, 0.9238795325112867385, 1.000000000000000000, 0.9238795325112866275, 1.000000000000000222 ) ) 
 REPRESENTATION_ITEM ( '' )  );
#11897 = CARTESIAN_POINT ( 'NONE',  ( -25.00000000000000000, 445.0000000000000568, -95.00000000000000000 ) ) ;
#11898 = CARTESIAN_POINT ( 'NONE',  ( 0.2500000000000002220, 0.000000000000000000, 4.000000000000000000 ) ) ;
#11899 = DIRECTION ( 'NONE',  ( 1.000000000000000000, -1.040834085586083310E-14, 0.000000000000000000 ) ) ;
#11900 = CARTESIAN_POINT ( 'NONE',  ( 165.0000000000011369, 230.0000000000000853, -20.00000000000000000 ) ) ;
#11901 = CARTESIAN_POINT ( 'NONE',  ( -2.708734125000000326, 112.8124999986344079, 3.317242575922457132E-16 ) ) ;
#11902 = CARTESIAN_POINT ( 'NONE',  ( -30.00000000000004263, 65.00000000000000000, 57.08203932499370836 ) ) ;
#11903 = CARTESIAN_POINT ( 'NONE',  ( 0.000000000000000000, -1.178949249685214307, 2.042000000000001592 ) ) ;
#11904 = EDGE_LOOP ( 'NONE', ( #11850, #5632, #12102, #10210 ) ) ;
#11905 = DIRECTION ( 'NONE',  ( 0.000000000000000000, 0.000000000000000000, -1.000000000000000000 ) ) ;
#11906 = ORIENTED_EDGE ( 'NONE', *, *, #405, .T. ) ;
#11907 = DIRECTION ( 'NONE',  ( 0.000000000000000000, 0.000000000000000000, -1.000000000000000000 ) ) ;
#11908 = CARTESIAN_POINT ( 'NONE',  ( 5.381387654344468530, 41.21666358253047946, 80.00000000000000000 ) ) ;
#11909 = ORIENTED_EDGE ( 'NONE', *, *, #3072, .F. ) ;
#11910 = DIRECTION ( 'NONE',  ( -0.000000000000000000, -1.000000000000000000, -0.000000000000000000 ) ) ;
#11911 = LINE ( 'NONE', #6294, #3612 ) ;
#11912 = ORIENTED_EDGE ( 'NONE', *, *, #5905, .T. ) ;
#11913 = CARTESIAN_POINT ( 'NONE',  ( 72.45442684796221045, 50.00000000000009237, -19.38521145883885666 ) ) ;
#11914 = AXIS2_PLACEMENT_3D ( 'NONE', #2674, #754, #9331 ) ;
#11915 = EDGE_CURVE ( 'NONE', #3006, #6671, #8278, .T. ) ;
#11916 = EDGE_CURVE ( 'NONE', #2084, #6749, #7355, .T. ) ;
#11917 = ORIENTED_EDGE ( 'NONE', *, *, #5597, .F. ) ;
#11918 = DIRECTION ( 'NONE',  ( 0.000000000000000000, 0.000000000000000000, 1.000000000000000000 ) ) ;
#11919 = EDGE_CURVE ( 'NONE', #3768, #1236, #3788, .T. ) ;
#11920 = CARTESIAN_POINT ( 'NONE',  ( -1.190781129305471087, 30.00000000000008882, 65.00000000000000000 ) ) ;
#11921 = ORIENTED_EDGE ( 'NONE', *, *, #10770, .F. ) ;
#11922 = FACE_OUTER_BOUND ( 'NONE', #4421, .T. ) ;
#11923 = DIRECTION ( 'NONE',  ( 0.000000000000000000, 0.000000000000000000, 1.000000000000000000 ) ) ;
#11924 = VECTOR ( 'NONE', #467, 1000.000000000000114 ) ;
#11925 = EDGE_LOOP ( 'NONE', ( #624, #636, #2250, #8401, #1923, #8679, #2145, #5268, #10351, #12056, #7724, #12133, #2000, #11376, #3377, #4133, #5381, #7598, #1984, #1931, #2216, #6367, #7471, #5724, #8111, #2435, #2126, #3512, #11719, #7915, #11978, #10922, #11664 ) ) ;
#11926 = DIRECTION ( 'NONE',  ( -0.000000000000000000, -1.000000000000000000, -0.000000000000000000 ) ) ;
#11927 = LINE ( 'NONE', #4072, #3525 ) ;
#11928 = DIRECTION ( 'NONE',  ( -0.5000000000000006661, -0.8660254037844383745, 0.000000000000000000 ) ) ;
#11929 = ORIENTED_EDGE ( 'NONE', *, *, #8128, .F. ) ;
#11930 = DIRECTION ( 'NONE',  ( 0.000000000000000000, 0.000000000000000000, 1.000000000000000000 ) ) ;
#11931 = CARTESIAN_POINT ( 'NONE',  ( 75.73945001075399830, 15.90984549754468524, 22.88037593554966165 ) ) ;
#11932 = AXIS2_PLACEMENT_3D ( 'NONE', #7307, #881, #10405 ) ;
#11933 = ORIENTED_EDGE ( 'NONE', *, *, #1240, .F. ) ;
#11934 = CARTESIAN_POINT ( 'NONE',  ( 75.20175883194669098, 16.56455603843833657, 23.64678730934253537 ) ) ;
#11935 = PLANE ( 'NONE',  #496 ) ;
#11936 = ORIENTED_EDGE ( 'NONE', *, *, #11154, .F. ) ;
#11937 = CARTESIAN_POINT ( 'NONE',  ( 25.00000000000000000, 445.0000000000000568, -24.99999999999998934 ) ) ;
#11938 = CARTESIAN_POINT ( 'NONE',  ( 74.58021194344081550, 42.25882445080058147, 24.47298709600845612 ) ) ;
#11939 = ORIENTED_EDGE ( 'NONE', *, *, #1886, .T. ) ;
#11940 = CARTESIAN_POINT ( 'NONE',  ( 0.000000000000000000, 170.0000000000000000, 0.000000000000000000 ) ) ;
#11941 = CARTESIAN_POINT ( 'NONE',  ( 1.121994411437819084, 112.4999999986343937, 2.708734125000000326 ) ) ;
#11942 = AXIS2_PLACEMENT_3D ( 'NONE', #1781, #11325, #6580 ) ;
#11943 = ORIENTED_EDGE ( 'NONE', *, *, #12131, .T. ) ;
#11944 = ORIENTED_EDGE ( 'NONE', *, *, #9367, .F. ) ;
#11945 = EDGE_CURVE ( 'NONE', #4047, #4313, #6184, .T. ) ;
#11946 = CIRCLE ( 'NONE', #6568, 3.250000000000000444 ) ;
#11947 = CARTESIAN_POINT ( 'NONE',  ( 3.061616997868383043E-15, 264.9990000000000236, -84.99999999999998579 ) ) ;
#11948 = EDGE_CURVE ( 'NONE', #3208, #5427, #1118, .T. ) ;
#11949 = CARTESIAN_POINT ( 'NONE',  ( -31.65330186654243505, 85.26794919243110371, -9.660254037844431707 ) ) ;
#11950 = CARTESIAN_POINT ( 'NONE',  ( 29.63582346253862454, 77.00000000000000000, -4.660254037844413944 ) ) ;
#11951 = CYLINDRICAL_SURFACE ( 'NONE', #5811, 125.0000000000000284 ) ;
#11952 = DIRECTION ( 'NONE',  ( 0.9595199576812829534, 0.000000000000000000, -0.2816406412634883671 ) ) ;
#11953 = LINE ( 'NONE', #3224, #5906 ) ;
#11954 = DIRECTION ( 'NONE',  ( -1.224646799147352961E-16, 0.000000000000000000, 1.000000000000000000 ) ) ;
#11955 = CARTESIAN_POINT ( 'NONE',  ( 69.76162866618028602, 16.50146430099879780, -27.53780242413600732 ) ) ;
#11956 = CARTESIAN_POINT ( 'NONE',  ( 3.250000000000000444, 110.0624999999999858, 1.346194077712559389 ) ) ;
#11957 = CIRCLE ( 'NONE', #3985, 9.999999999999994671 ) ;
#11958 = ORIENTED_EDGE ( 'NONE', *, *, #8645, .T. ) ;
#11959 = DIRECTION ( 'NONE',  ( 0.000000000000000000, 0.000000000000000000, 1.000000000000000000 ) ) ;
#11960 = ADVANCED_FACE ( 'NONE', ( #5794 ), #2985, .T. ) ;
#11961 = ORIENTED_EDGE ( 'NONE', *, *, #5548, .F. ) ;
#11962 = AXIS2_PLACEMENT_3D ( 'NONE', #10364, #2761, #3578 ) ;
#11963 = CIRCLE ( 'NONE', #6585, 5.000000000000001776 ) ;
#11964 = LINE ( 'NONE', #10955, #7225 ) ;
#11965 = EDGE_LOOP ( 'NONE', ( #2394, #3764, #7029, #1047 ) ) ;
#11966 = CIRCLE ( 'NONE', #3596, 24.99999999999999645 ) ;
#11967 = CARTESIAN_POINT ( 'NONE',  ( 77.45966692414835109, 45.00000000000008527, -20.00000000000000000 ) ) ;
#11968 = CARTESIAN_POINT ( 'NONE',  ( 75.70364277637115435, 15.94008215020948427, -22.93512150616605183 ) ) ;
#11969 = VERTEX_POINT ( 'NONE', #7836 ) ;
#11970 = CARTESIAN_POINT ( 'NONE',  ( 0.000000000000000000, 0.000000000000000000, 4.000000000000000000 ) ) ;
#11971 = DIRECTION ( 'NONE',  ( 0.000000000000000000, -1.000000000000000000, 0.000000000000000000 ) ) ;
#11972 = VERTEX_POINT ( 'NONE', #3856 ) ;
#11973 = CARTESIAN_POINT ( 'NONE',  ( 25.00000000000000355, 570.2996408614167194, -90.00000000000000000 ) ) ;
#11974 = AXIS2_PLACEMENT_3D ( 'NONE', #11108, #9852, #2445 ) ;
#11975 = CIRCLE ( 'NONE', #826, 35.00000000000000000 ) ;
#11976 = EDGE_CURVE ( 'NONE', #7882, #10309, #5395, .T. ) ;
#11977 = EDGE_CURVE ( 'NONE', #6060, #108, #1801, .T. ) ;
#11978 = ORIENTED_EDGE ( 'NONE', *, *, #643, .F. ) ;
#11979 = ORIENTED_EDGE ( 'NONE', *, *, #968, .T. ) ;
#11980 = CIRCLE ( 'NONE', #7396, 15.00000000000000000 ) ;
#11981 = CARTESIAN_POINT ( 'NONE',  ( 30.08147999331295352, 76.80445198238156479, -4.520396356853239261 ) ) ;
#11982 = CARTESIAN_POINT ( 'NONE',  ( -5.970153145843347347E-16, 114.6249999972688158, -3.250000000000000444 ) ) ;
#11983 = EDGE_LOOP ( 'NONE', ( #4509, #7380, #4733, #1255, #7045, #3327, #7631 ) ) ;
#11984 = VERTEX_POINT ( 'NONE', #1986 ) ;
#11985 = CARTESIAN_POINT ( 'NONE',  ( -107.1104145097476987, 285.0000000000000568, 41.86118851095882576 ) ) ;
#11986 = CARTESIAN_POINT ( 'NONE',  ( 71.22480170918207421, 11.35480001874193690, 23.50133972577969743 ) ) ;
#11987 = CIRCLE ( 'NONE', #2815, 2.041999999999999815 ) ;
#11988 = VERTEX_POINT ( 'NONE', #169 ) ;
#11989 = CARTESIAN_POINT ( 'NONE',  ( 3.980102097228898231E-16, 115.0000000000000000, -3.250000000000000444 ) ) ;
#11990 = LINE ( 'NONE', #5374, #1342 ) ;
#11991 = ORIENTED_EDGE ( 'NONE', *, *, #4636, .F. ) ;
#11992 = DIRECTION ( 'NONE',  ( 1.000000000000000000, -0.000000000000000000, 1.224646799147353207E-16 ) ) ;
#11993 = CARTESIAN_POINT ( 'NONE',  ( 70.44139041661959766, 13.32009519262272690, 25.75312943552223643 ) ) ;
#11994 = VECTOR ( 'NONE', #978, 1000.000000000000000 ) ;
#11995 = ORIENTED_EDGE ( 'NONE', *, *, #12299, .F. ) ;
#11996 = DIRECTION ( 'NONE',  ( 1.000000000000000000, 0.000000000000000000, -0.000000000000000000 ) ) ;
#11997 = DIRECTION ( 'NONE',  ( 0.000000000000000000, 1.000000000000000000, 0.000000000000000000 ) ) ;
#11998 = ORIENTED_EDGE ( 'NONE', *, *, #4088, .T. ) ;
#11999 = CARTESIAN_POINT ( 'NONE',  ( -31.74999999999995737, 5.204748896376250699E-16, -4.250000000000000000 ) ) ;
#12000 = CARTESIAN_POINT ( 'NONE',  ( 76.19870213673728188, 44.50753802327100317, 22.18755841417295827 ) ) ;
#12001 = EDGE_LOOP ( 'NONE', ( #8891, #10076, #5243, #4407 ) ) ;
#12002 = CARTESIAN_POINT ( 'NONE',  ( 0.000000000000000000, 87.50000000000000000, 24.99999999999999645 ) ) ;
#12003 = EDGE_CURVE ( 'NONE', #2376, #11519, #7893, .T. ) ;
#12004 = DIRECTION ( 'NONE',  ( -0.000000000000000000, -1.000000000000000000, -0.000000000000000000 ) ) ;
#12005 = CARTESIAN_POINT ( 'NONE',  ( 1.658621287961228566E-16, 113.5624999986344079, 2.708734125000000326 ) ) ;
#12006 = ORIENTED_EDGE ( 'NONE', *, *, #6789, .T. ) ;
#12007 =( LENGTH_UNIT ( ) NAMED_UNIT ( * ) SI_UNIT ( .MILLI., .METRE. ) );
#12008 = ORIENTED_EDGE ( 'NONE', *, *, #2732, .F. ) ;
#12009 = AXIS2_PLACEMENT_3D ( 'NONE', #7660, #10650, #6728 ) ;
#12010 = PLANE ( 'NONE',  #8828 ) ;
#12011 = CARTESIAN_POINT ( 'NONE',  ( 165.0000000000011369, 37.07106781186552524, -25.00000000000000000 ) ) ;
#12012 = DIRECTION ( 'NONE',  ( 0.000000000000000000, 0.000000000000000000, 1.000000000000000000 ) ) ;
#12013 = CARTESIAN_POINT ( 'NONE',  ( 0.000000000000000000, 275.0000000000000000, 0.000000000000000000 ) ) ;
#12014 = CARTESIAN_POINT ( 'NONE',  ( -12.32411137850302119, 23.28349364905396612, 79.50000000000000000 ) ) ;
#12015 = CARTESIAN_POINT ( 'NONE',  ( 34.31149098582250190, 75.26794919243110371, -7.660254037844446806 ) ) ;
#12016 = ADVANCED_FACE ( 'NONE', ( #8766 ), #3106, .T. ) ;
#12017 = CARTESIAN_POINT ( 'NONE',  ( -6.000000000000000000, 62.00000000000000000, 70.00000000000001421 ) ) ;
#12018 = CARTESIAN_POINT ( 'NONE',  ( -5.970153145843347347E-16, 111.6249999972688158, -3.250000000000000444 ) ) ;
#12019 = CARTESIAN_POINT ( 'NONE',  ( 1.990051048614449116E-16, 111.2500000000000000, 3.250000000000000444 ) ) ;
#12020 = VECTOR ( 'NONE', #8570, 1000.000000000000000 ) ;
#12021 = ADVANCED_FACE ( 'NONE', ( #10702 ), #8825, .F. ) ;
#12022 = CARTESIAN_POINT ( 'NONE',  ( 17.30235457177317571, 275.0000000000000000, -113.6909342308024407 ) ) ;
#12023 = ORIENTED_EDGE ( 'NONE', *, *, #3762, .T. ) ;
#12024 = AXIS2_PLACEMENT_3D ( 'NONE', #10941, #10883, #283 ) ;
#12025 = DIRECTION ( 'NONE',  ( -0.000000000000000000, -0.000000000000000000, 1.000000000000000000 ) ) ;
#12026 = ORIENTED_EDGE ( 'NONE', *, *, #3541, .F. ) ;
#12027 = VECTOR ( 'NONE', #3766, 1000.000000000000227 ) ;
#12028 = DIRECTION ( 'NONE',  ( 0.000000000000000000, 0.000000000000000000, 1.000000000000000000 ) ) ;
#12029 = DIRECTION ( 'NONE',  ( -0.000000000000000000, -1.000000000000000000, 0.000000000000000000 ) ) ;
#12030 = VERTEX_POINT ( 'NONE', #5854 ) ;
#12031 = PLANE ( 'NONE',  #4874 ) ;
#12032 = CARTESIAN_POINT ( 'NONE',  ( 1.990051048614449116E-16, 111.1249999972688158, 3.250000000000000444 ) ) ;
#12033 = EDGE_CURVE ( 'NONE', #7550, #1521, #1237, .T. ) ;
#12034 = ADVANCED_FACE ( 'NONE', ( #7719 ), #10584, .T. ) ;
#12035 = ORIENTED_EDGE ( 'NONE', *, *, #10642, .T. ) ;
#12036 = DIRECTION ( 'NONE',  ( -0.000000000000000000, -1.000000000000000000, -0.000000000000000000 ) ) ;
#12037 = VECTOR ( 'NONE', #8605, 999.9999999999997726 ) ;
#12038 = AXIS2_PLACEMENT_3D ( 'NONE', #11152, #12279, #1795 ) ;
#12039 = EDGE_LOOP ( 'NONE', ( #10523, #3030, #998 ) ) ;
#12040 = CARTESIAN_POINT ( 'NONE',  ( -7.690781129305457320, 18.74166975080245834, 80.00000000000000000 ) ) ;
#12041 = CARTESIAN_POINT ( 'NONE',  ( 2.979367062500000163, 110.1562499993171969, 0.000000000000000000 ) ) ;
#12042 = VERTEX_POINT ( 'NONE', #11712 ) ;
#12043 = CARTESIAN_POINT ( 'NONE',  ( 30.00100000000000122, 77.00000000000000000, 8.660254037844445918 ) ) ;
#12044 = FACE_OUTER_BOUND ( 'NONE', #6923, .T. ) ;
#12045 = VERTEX_POINT ( 'NONE', #3163 ) ;
#12046 = ADVANCED_FACE ( 'NONE', ( #9637 ), #43, .F. ) ;
#12047 = CARTESIAN_POINT ( 'NONE',  ( 9.184850993605151889E-15, 65.00000000000000000, 75.00000000000002842 ) ) ;
#12048 = VECTOR ( 'NONE', #10542, 1000.000000000000000 ) ;
#12049 = CARTESIAN_POINT ( 'NONE',  ( -27.31079997599232456, 86.91362087007181003, -12.41453806599178655 ) ) ;
#12050 = DIRECTION ( 'NONE',  ( -0.000000000000000000, 1.000000000000000000, 0.000000000000000000 ) ) ;
#12051 = ORIENTED_EDGE ( 'NONE', *, *, #1773, .F. ) ;
#12052 = CARTESIAN_POINT ( 'NONE',  ( -1.190781129305471087, 30.00000000000008882, 80.00000000000000000 ) ) ;
#12053 = CYLINDRICAL_SURFACE ( 'NONE', #11577, 100.0000000000000142 ) ;
#12054 = VECTOR ( 'NONE', #987, 1000.000000000000000 ) ;
#12055 = VECTOR ( 'NONE', #4868, 1000.000000000000000 ) ;
#12056 = ORIENTED_EDGE ( 'NONE', *, *, #11334, .F. ) ;
#12057 = DIRECTION ( 'NONE',  ( 0.000000000000000000, 0.000000000000000000, 1.000000000000000000 ) ) ;
#12058 = CYLINDRICAL_SURFACE ( 'NONE', #1497, 3.250000000000000444 ) ;
#12059 = ORIENTED_EDGE ( 'NONE', *, *, #10184, .F. ) ;
#12060 = DIRECTION ( 'NONE',  ( -0.000000000000000000, -1.000000000000000000, -0.000000000000000000 ) ) ;
#12061 = LINE ( 'NONE', #8360, #3697 ) ;
#12062 = VERTEX_POINT ( 'NONE', #2114 ) ;
#12063 = DIRECTION ( 'NONE',  ( 0.000000000000000000, 0.000000000000000000, 1.000000000000000000 ) ) ;
#12064 = AXIS2_PLACEMENT_3D ( 'NONE', #6649, #1848, #5601 ) ;
#12065 = CARTESIAN_POINT ( 'NONE',  ( 3.592712519748626931, 21.21474596215575659, 79.50000000000000000 ) ) ;
#12066 = CARTESIAN_POINT ( 'NONE',  ( -2.708734125000000326, 112.8124999986344079, 3.317242575922457132E-16 ) ) ;
#12067 = AXIS2_PLACEMENT_3D ( 'NONE', #5967, #10885, #1292 ) ;
#12068 = CARTESIAN_POINT ( 'NONE',  ( -1.915364268218909594, 113.1874999986344079, -1.915364268218908927 ) ) ;
#12069 = ORIENTED_EDGE ( 'NONE', *, *, #2721, .F. ) ;
#12070 = ORIENTED_EDGE ( 'NONE', *, *, #10868, .T. ) ;
#12071 = CLOSED_SHELL ( 'NONE', ( #9280, #2466, #6770, #6104, #3969, #1741 ) ) ;
#12072 =( LENGTH_UNIT ( ) NAMED_UNIT ( * ) SI_UNIT ( .MILLI., .METRE. ) );
#12073 = CIRCLE ( 'NONE', #3504, 70.00000000000001421 ) ;
#12074 = ADVANCED_FACE ( 'NONE', ( #5915 ), #9700, .F. ) ;
#12075 = EDGE_CURVE ( 'NONE', #6884, #11798, #5229, .T. ) ;
#12076 = AXIS2_PLACEMENT_3D ( 'NONE', #7115, #1507, #503 ) ;
#12077 = CARTESIAN_POINT ( 'NONE',  ( 11.80921887069467324, 30.25000000000018474, 80.00000000000000000 ) ) ;
#12078 = DIRECTION ( 'NONE',  ( 0.000000000000000000, 0.000000000000000000, -1.000000000000000000 ) ) ;
#12080 = ADVANCED_FACE ( 'NONE', ( #11780 ), #10556, .T. ) ;
#12079 = CARTESIAN_POINT ( 'NONE',  ( 10.06754911989234635, 23.50000000000004974, 80.00000000000000000 ) ) ;
#12081 = DIRECTION ( 'NONE',  ( -0.8660254037844432595, 0.000000000000000000, 0.4999999999999920064 ) ) ;
#12082 = DIRECTION ( 'NONE',  ( 0.8660254037844434816, 0.4999999999999913958, 0.000000000000000000 ) ) ;
#12083 = CARTESIAN_POINT ( 'NONE',  ( 0.000000000000000000, 75.00000000000000000, 25.00000000000000000 ) ) ;
#12084 = CARTESIAN_POINT ( 'NONE',  ( 13.78766650650841186, 29.07005748252881361, 73.72178925532224980 ) ) ;
#12085 = CARTESIAN_POINT ( 'NONE',  ( 3.250000000000000444, 111.8749999972688158, 0.000000000000000000 ) ) ;
#12086 = ORIENTED_EDGE ( 'NONE', *, *, #7597, .F. ) ;
#12087 = CARTESIAN_POINT ( 'NONE',  ( -5.970153145843347347E-16, 111.7500000000000000, -3.250000000000000444 ) ) ;
#12088 = DIRECTION ( 'NONE',  ( -0.000000000000000000, 1.000000000000000000, -0.000000000000000000 ) ) ;
#12089 = AXIS2_PLACEMENT_3D ( 'NONE', #1768, #7505, #5521 ) ;
#12090 = CARTESIAN_POINT ( 'NONE',  ( 0.000000000000000000, 10.00000000000017586, 75.00000000000001421 ) ) ;
#12091 = ORIENTED_EDGE ( 'NONE', *, *, #1222, .T. ) ;
#12092 = DIRECTION ( 'NONE',  ( -0.000000000000000000, -1.000000000000000000, -0.000000000000000000 ) ) ;
#12093 = DIRECTION ( 'NONE',  ( 1.000000000000000000, 0.000000000000000000, 0.000000000000000000 ) ) ;
#12094 = DIRECTION ( 'NONE',  ( 0.000000000000000000, 0.000000000000000000, 1.000000000000000000 ) ) ;
#12095 = ORIENTED_EDGE ( 'NONE', *, *, #3285, .F. ) ;
#12096 = CARTESIAN_POINT ( 'NONE',  ( 3.980102097228898231E-16, 110.0000000000000000, -3.250000000000000444 ) ) ;
#12097 = CIRCLE ( 'NONE', #4522, 30.00000000000000000 ) ;
#12098 = CARTESIAN_POINT ( 'NONE',  ( 0.000000000000000000, 15.00000000000008882, 0.000000000000000000 ) ) ;
#12099 = ORIENTED_EDGE ( 'NONE', *, *, #12033, .T. ) ;
#12100 = CARTESIAN_POINT ( 'NONE',  ( 0.000000000000000000, 1.178949249685217415, 2.041999999999998483 ) ) ;
#12101 = ADVANCED_FACE ( 'NONE', ( #418 ), #480, .T. ) ;
#12102 = ORIENTED_EDGE ( 'NONE', *, *, #2279, .T. ) ;
#12103 = EDGE_CURVE ( 'NONE', #2554, #11257, #8362, .T. ) ;
#12104 = CARTESIAN_POINT ( 'NONE',  ( 34.80906958247980754, 75.85155757747834571, -7.997200496052795593 ) ) ;
#12106 = VERTEX_POINT ( 'NONE', #3355 ) ;
#12105 = CARTESIAN_POINT ( 'NONE',  ( 117.9289321881355193, 40.00000000000009237, -20.00000000000000000 ) ) ;
#12107 = VERTEX_POINT ( 'NONE', #7152 ) ;
#12108 = LINE ( 'NONE', #10634, #6407 ) ;
#12109 = CARTESIAN_POINT ( 'NONE',  ( -30.03968734988933420, 77.39454232463201322, 4.824121477407818048 ) ) ;
#12110 = ORIENTED_EDGE ( 'NONE', *, *, #7393, .F. ) ;
#12111 = DIRECTION ( 'NONE',  ( 0.000000000000000000, 1.000000000000000000, 0.000000000000000000 ) ) ;
#12112 = DIRECTION ( 'NONE',  ( 0.000000000000000000, 0.000000000000000000, 1.000000000000000000 ) ) ;
#12113 = ORIENTED_EDGE ( 'NONE', *, *, #5036, .T. ) ;
#12114 = CARTESIAN_POINT ( 'NONE',  ( -1.915364268218908927, 113.9374999986344079, 1.915364268218909150 ) ) ;
#12115 = DIRECTION ( 'NONE',  ( -0.8660254037844377084, 0.5000000000000015543, 0.000000000000000000 ) ) ;
#12116 =( REPRESENTATION_RELATIONSHIP ('NONE','NONE', #3713, #3316 ) REPRESENTATION_RELATIONSHIP_WITH_TRANSFORMATION ( #7665 )SHAPE_REPRESENTATION_RELATIONSHIP( ) );
#12117 = EDGE_CURVE ( 'NONE', #2446, #3205, #8761, .T. ) ;
#12118 = ADVANCED_FACE ( 'NONE', ( #8015 ), #8137, .T. ) ;
#12119 = VERTEX_POINT ( 'NONE', #2480 ) ;
#12120 = VECTOR ( 'NONE', #9641, 1000.000000000000114 ) ;
#12121 = FACE_OUTER_BOUND ( 'NONE', #1485, .T. ) ;
#12122 = CARTESIAN_POINT ( 'NONE',  ( 70.88057259133860555, 47.89215595910781786, 24.51542725512078746 ) ) ;
#12123 = ORIENTED_EDGE ( 'NONE', *, *, #3925, .F. ) ;
#12124 = FACE_OUTER_BOUND ( 'NONE', #4292, .T. ) ;
#12125 = FACE_OUTER_BOUND ( 'NONE', #230, .T. ) ;
#12126 = ORIENTED_EDGE ( 'NONE', *, *, #4197, .T. ) ;
#12127 = CARTESIAN_POINT ( 'NONE',  ( 8.572527594031474570E-15, 65.00000000000000000, 70.00000000000001421 ) ) ;
#12128 = DIRECTION ( 'NONE',  ( -0.000000000000000000, -1.000000000000000000, -0.000000000000000000 ) ) ;
#12129 = PLANE ( 'NONE',  #10157 ) ;
#12130 = CARTESIAN_POINT ( 'NONE',  ( 2.708734124999999882, 112.5624999986344079, 0.000000000000000000 ) ) ;
#12131 = EDGE_CURVE ( 'NONE', #9447, #4650, #1297, .T. ) ;
#12132 = ORIENTED_EDGE ( 'NONE', *, *, #12299, .T. ) ;
#12133 = ORIENTED_EDGE ( 'NONE', *, *, #5948, .T. ) ;
#12134 = EDGE_CURVE ( 'NONE', #9665, #8933, #7385, .T. ) ;
#12135 = EDGE_CURVE ( 'NONE', #7067, #11423, #10827, .T. ) ;
#12136 = DIRECTION ( 'NONE',  ( 0.000000000000000000, 0.000000000000000000, -1.000000000000000000 ) ) ;
#12137 = DIRECTION ( 'NONE',  ( 0.000000000000000000, 1.000000000000000000, 0.000000000000000000 ) ) ;
#12138 = CARTESIAN_POINT ( 'NONE',  ( -32.61619934561887391, 76.99999999999998579, 8.120688671832020589 ) ) ;
#12139 = DIRECTION ( 'NONE',  ( 0.000000000000000000, 0.000000000000000000, -1.000000000000000000 ) ) ;
#12140 = B_SPLINE_CURVE_WITH_KNOTS ( 'NONE', 3,
 ( #6296, #6235, #11795, #1560, #10966, #3369, #3240, #7042, #5362, #10841, #2303, #6114, #1373, #8027, #5241, #555, #10903, #9019, #3435, #495, #10025, #8091, #11913, #4352 ),
 .UNSPECIFIED., .F., .F.,
 ( 4, 2, 2, 2, 2, 2, 2, 2, 2, 2, 2, 4 ),
 ( 0.000000000000000000, 0.0009796746052620941732, 0.001959349210524188346, 0.003918698421048397509, 0.004898373026310511198, 0.005878047631572623152, 0.007837396842096862673, 0.009796746052621102194, 0.01175609526314533824, 0.01273576986840745454, 0.01371544447366956909, 0.01567479368419381555 ),
 .UNSPECIFIED. ) ;
#12141 = DIRECTION ( 'NONE',  ( 0.000000000000000000, 0.000000000000000000, 1.000000000000000000 ) ) ;
#12142 = CARTESIAN_POINT ( 'NONE',  ( -0.9407811293054709756, 40.00000000000008527, 79.50000000000000000 ) ) ;
#12143 = CARTESIAN_POINT ( 'NONE',  ( -7.474274778359198734, 41.38333024919781167, 79.50000000000000000 ) ) ;
#12144 = CARTESIAN_POINT ( 'NONE',  ( -5.970153145843347347E-16, 113.7500000000000000, -3.250000000000000444 ) ) ;
#12145 = ADVANCED_FACE ( 'NONE', ( #5167, #8945 ), #10071, .T. ) ;
#12146 = FACE_OUTER_BOUND ( 'NONE', #10295, .T. ) ;
#12147 = AXIS2_PLACEMENT_3D ( 'NONE', #4416, #5122, #6048 ) ;
#12148 = AXIS2_PLACEMENT_3D ( 'NONE', #3940, #7738, #6621 ) ;
#12149 = DIRECTION ( 'NONE',  ( 0.000000000000000000, 0.000000000000000000, -1.000000000000000000 ) ) ;
#12150 = VERTEX_POINT ( 'NONE', #6282 ) ;
#12151 = FACE_OUTER_BOUND ( 'NONE', #2006, .T. ) ;
#12152 = CARTESIAN_POINT ( 'NONE',  ( 0.000000000000000000, 122.5000000000000000, 0.000000000000000000 ) ) ;
#12153 = FACE_OUTER_BOUND ( 'NONE', #9276, .T. ) ;
#12154 = ORIENTED_EDGE ( 'NONE', *, *, #5488, .T. ) ;
#12155 = CIRCLE ( 'NONE', #5782, 45.00000000000000000 ) ;
#12156 = CARTESIAN_POINT ( 'NONE',  ( -12.32202939415814846, 23.28469568327592754, 80.00000000000000000 ) ) ;
#12157 = ADVANCED_FACE ( 'NONE', ( #2411 ), #10361, .F. ) ;
#12158 = CARTESIAN_POINT ( 'NONE',  ( 0.000000000000000000, 345.0000000000000568, 110.0000000000000284 ) ) ;
#12159 = ORIENTED_EDGE ( 'NONE', *, *, #956, .F. ) ;
#12160 = DIRECTION ( 'NONE',  ( 1.000000000000000000, 0.000000000000000000, 0.000000000000000000 ) ) ;
#12161 = AXIS2_PLACEMENT_3D ( 'NONE', #1620, #4482, #10208 ) ;
#12162 = AXIS2_PLACEMENT_3D ( 'NONE', #4527, #732, #8315 ) ;
#12163 = EDGE_LOOP ( 'NONE', ( #11060, #3863, #7053, #2380, #8604, #6519 ) ) ;
#12164 = CARTESIAN_POINT ( 'NONE',  ( 0.000000000000000000, 75.00000000000001421, 25.00000000000000000 ) ) ;
#12166 = ORIENTED_EDGE ( 'NONE', *, *, #2975, .F. ) ;
#12165 = CARTESIAN_POINT ( 'NONE',  ( 0.000000000000000000, 165.5000000000000000, 0.000000000000000000 ) ) ;
#12167 = EDGE_LOOP ( 'NONE', ( #11995, #9874, #5139, #8957 ) ) ;
#12168 = DIRECTION ( 'NONE',  ( 0.9682458365518540333, 0.000000000000000000, -0.2500000000000003331 ) ) ;
#12169 = DIRECTION ( 'NONE',  ( 0.000000000000000000, 0.000000000000000000, 1.000000000000000000 ) ) ;
#12170 = ORIENTED_EDGE ( 'NONE', *, *, #9839, .T. ) ;
#12171 = CARTESIAN_POINT ( 'NONE',  ( -3.061616997868391523E-16, 175.0000000000000284, 0.000000000000000000 ) ) ;
#12172 = PLANE ( 'NONE',  #4454 ) ;
#12174 = DIRECTION ( 'NONE',  ( 0.000000000000000000, 1.000000000000000000, 0.000000000000000000 ) ) ;
#12173 = VECTOR ( 'NONE', #5153, 999.9999999999998863 ) ;
#12175 = DIRECTION ( 'NONE',  ( -0.5000000000000036637, -0.8660254037844365982, 0.000000000000000000 ) ) ;
#12176 = ORIENTED_EDGE ( 'NONE', *, *, #9647, .T. ) ;
#12177 = CARTESIAN_POINT ( 'NONE',  ( -2.708734124999999882, 110.9999999986343937, 1.121994411437818862 ) ) ;
#12178 = EDGE_CURVE ( 'NONE', #8994, #4082, #10891, .T. ) ;
#12179 = CARTESIAN_POINT ( 'NONE',  ( 70.79098555864042908, 20.00000000000009237, 25.00000000000000000 ) ) ;
#12180 = EDGE_CURVE ( 'NONE', #5955, #9853, #10756, .T. ) ;
#12181 = VECTOR ( 'NONE', #4780, 1000.000000000000000 ) ;
#12182 = VECTOR ( 'NONE', #1435, 1000.000000000000000 ) ;
#12183 = ORIENTED_EDGE ( 'NONE', *, *, #4193, .F. ) ;
#12184 = CARTESIAN_POINT ( 'NONE',  ( 1.990051048614449116E-16, 113.2500000000000000, 3.250000000000000444 ) ) ;
#12185 = CARTESIAN_POINT ( 'NONE',  ( 70.26686370603786713, 46.04793283185657060, 26.22231631056804346 ) ) ;
#12186 = VERTEX_POINT ( 'NONE', #1482 ) ;
#12187 = LINE ( 'NONE', #8541, #5469 ) ;
#12188 = CARTESIAN_POINT ( 'NONE',  ( -1.190781129305471087, 30.00000000000008882, 80.00000000000000000 ) ) ;
#12189 = VERTEX_POINT ( 'NONE', #2348 ) ;
#12190 = CARTESIAN_POINT ( 'NONE',  ( -25.00000000000000000, 570.2996408614167194, -90.00000000000000000 ) ) ;
#12191 = DIRECTION ( 'NONE',  ( -0.8660254037844394848, -0.4999999999999985012, 0.000000000000000000 ) ) ;
#12192 = AXIS2_PLACEMENT_3D ( 'NONE', #1170, #9692, #4972 ) ;
#12193 = CARTESIAN_POINT ( 'NONE',  ( 1.658621287961228320E-16, 113.8124999986344079, 2.708734124999999882 ) ) ;
#12194 = EDGE_CURVE ( 'NONE', #10639, #11257, #6155, .T. ) ;
#12195 = PLANE ( 'NONE',  #11068 ) ;
#12196 = ORIENTED_EDGE ( 'NONE', *, *, #11024, .F. ) ;
#12197 = VERTEX_POINT ( 'NONE', #1421 ) ;
#12198 = EDGE_CURVE ( 'NONE', #5570, #10546, #542, .T. ) ;
#12199 = DIRECTION ( 'NONE',  ( 0.000000000000000000, 1.000000000000000000, 0.000000000000000000 ) ) ;
#12200 = FACE_BOUND ( 'NONE', #11333, .T. ) ;
#12201 = CARTESIAN_POINT ( 'NONE',  ( -30.23169114332096896, 76.99999999999998579, 5.192055827170280580 ) ) ;
#12202 = DIRECTION ( 'NONE',  ( -1.000000000000000000, 0.000000000000000000, 0.000000000000000000 ) ) ;
#12203 = CARTESIAN_POINT ( 'NONE',  ( -14.19078112930533031, 30.00000000000017764, 80.00000000000000000 ) ) ;
#12204 = DIRECTION ( 'NONE',  ( 0.000000000000000000, 0.000000000000000000, 1.000000000000000000 ) ) ;
#12205 = DIRECTION ( 'NONE',  ( 0.000000000000000000, -0.000000000000000000, 1.000000000000000000 ) ) ;
#12206 = EDGE_CURVE ( 'NONE', #2842, #10602, #4467, .T. ) ;
#12207 = EDGE_CURVE ( 'NONE', #10533, #1040, #11963, .T. ) ;
#12208 = FACE_BOUND ( 'NONE', #4484, .T. ) ;
#12209 = CIRCLE ( 'NONE', #8797, 100.0000000000000284 ) ;
#12210 = DIRECTION ( 'NONE',  ( 0.000000000000000000, 1.000000000000000000, 0.000000000000000000 ) ) ;
#12211 = ORIENTED_EDGE ( 'NONE', *, *, #3717, .T. ) ;
#12212 = CARTESIAN_POINT ( 'NONE',  ( 29.63582346253862454, 77.00000000000000000, -4.660254037844413944 ) ) ;
#12213 = CARTESIAN_POINT ( 'NONE',  ( -6.000000000000000000, 50.00000000000000000, 70.00000000000001421 ) ) ;
#12214 = CARTESIAN_POINT ( 'NONE',  ( -12.49077804517044221, 23.57216878365009194, 80.00000000000000000 ) ) ;
#12215 = ORIENTED_EDGE ( 'NONE', *, *, #1836, .F. ) ;
#12216 = AXIS2_PLACEMENT_3D ( 'NONE', #1549, #4287, #5354 ) ;
#12217 = DIRECTION ( 'NONE',  ( -0.000000000000000000, -1.000000000000000000, -0.000000000000000000 ) ) ;
#12218 = CARTESIAN_POINT ( 'NONE',  ( 2.500000000000000000, -1.178949249685214307, 2.042000000000001592 ) ) ;
#12219 = VERTEX_POINT ( 'NONE', #11272 ) ;
#12220 = DIRECTION ( 'NONE',  ( -0.4999999999999970579, 0.8660254037844403729, 0.000000000000000000 ) ) ;
#12221 = VECTOR ( 'NONE', #5231, 1000.000000000000227 ) ;
#12222 = ADVANCED_FACE ( 'NONE', ( #8443 ), #6530, .F. ) ;
#12223 = ORIENTED_EDGE ( 'NONE', *, *, #338, .T. ) ;
#12224 = ADVANCED_FACE ( 'NONE', ( #8503 ), #7343, .T. ) ;
#12225 = DIRECTION ( 'NONE',  ( 0.000000000000000000, 0.000000000000000000, 1.000000000000000000 ) ) ;
#12227 = VERTEX_POINT ( 'NONE', #1731 ) ;
#12226 = DIRECTION ( 'NONE',  ( 0.000000000000000000, 0.000000000000000000, 1.000000000000000000 ) ) ;
#12228 = EDGE_LOOP ( 'NONE', ( #9452, #9456, #2315, #2798 ) ) ;
#12229 = CARTESIAN_POINT ( 'NONE',  ( 0.000000000000000000, 345.0000000000000568, -59.99999999999999289 ) ) ;
#12230 = ORIENTED_EDGE ( 'NONE', *, *, #9433, .T. ) ;
#12231 = ADVANCED_FACE ( 'NONE', ( #9190, #12208 ), #3715, .T. ) ;
#12232 = PRESENTATION_STYLE_ASSIGNMENT (( #8223 ) ) ;
#12233 = DIRECTION ( 'NONE',  ( 1.000000000000000000, 0.000000000000000000, -3.469446951953613696E-16 ) ) ;
#12234 = DIRECTION ( 'NONE',  ( 0.000000000000000000, 0.8660254037844407060, -0.4999999999999965028 ) ) ;
#12235 = DIRECTION ( 'NONE',  ( -0.000000000000000000, -1.000000000000000000, -0.000000000000000000 ) ) ;
#12236 = VECTOR ( 'NONE', #9801, 1000.000000000000227 ) ;
#12237 = AXIS2_PLACEMENT_3D ( 'NONE', #552, #2358, #4349 ) ;
#12238 = ORIENTED_EDGE ( 'NONE', *, *, #5321, .F. ) ;
#12239 = CARTESIAN_POINT ( 'NONE',  ( 2.708734125000000326, 110.3749999986344221, 1.121994411437818862 ) ) ;
#12240 = DIRECTION ( 'NONE',  ( -0.000000000000000000, -0.4999999999999974465, 0.8660254037844401509 ) ) ;
#12241 = VERTEX_POINT ( 'NONE', #10316 ) ;
#12242 = DIRECTION ( 'NONE',  ( -1.000000000000000000, 0.000000000000000000, 0.000000000000000000 ) ) ;
#12243 = CARTESIAN_POINT ( 'NONE',  ( -15.63313230619844241, 25.91538294882372995, 73.35278444408292842 ) ) ;
#12244 = SHAPE_REPRESENTATION ( 'Pulse _ Speed Control Dial', ( #1612 ), #4147 ) ;
#12245 = VERTEX_POINT ( 'NONE', #5474 ) ;
#12246 = AXIS2_PLACEMENT_3D ( 'NONE', #9634, #6596, #6720 ) ;
#12247 = FACE_OUTER_BOUND ( 'NONE', #11173, .T. ) ;
#12248 = LINE ( 'NONE', #6445, #1316 ) ;
#12249 = ORIENTED_EDGE ( 'NONE', *, *, #10617, .T. ) ;
#12250 = CARTESIAN_POINT ( 'NONE',  ( -13.00000000000000178, 170.0000000000000000, -7.483314773547880883 ) ) ;
#12251 = CARTESIAN_POINT ( 'NONE',  ( -8.500000000000000000, 216.0365690573663926, -7.483314773547880883 ) ) ;
#12252 = CARTESIAN_POINT ( 'NONE',  ( 3.249999999999999556, 114.8124999972688016, -1.346194077712561610 ) ) ;
#12253 = DIRECTION ( 'NONE',  ( 1.000000000000000000, 0.000000000000000000, 0.000000000000000000 ) ) ;
#12254 = CIRCLE ( 'NONE', #905, 75.00000000000001421 ) ;
#12255 = ORIENTED_EDGE ( 'NONE', *, *, #3334, .F. ) ;
#12256 =( NAMED_UNIT ( * ) SI_UNIT ( $, .STERADIAN. ) SOLID_ANGLE_UNIT ( ) );
#12257 = CIRCLE ( 'NONE', #2098, 25.00000000000000000 ) ;
#12258 = DIRECTION ( 'NONE',  ( -0.000000000000000000, -1.000000000000000000, -0.000000000000000000 ) ) ;
#12259 = ORIENTED_EDGE ( 'NONE', *, *, #2273, .T. ) ;
#12260 = ADVANCED_FACE ( 'NONE', ( #4711 ), #9255, .T. ) ;
#12261 = LINE ( 'NONE', #3708, #41 ) ;
#12262 = VECTOR ( 'NONE', #5340, 1000.000000000000000 ) ;
#12263 = DIRECTION ( 'NONE',  ( 1.000000000000000000, -0.000000000000000000, 1.224646799147353207E-16 ) ) ;
#12264 = DIRECTION ( 'NONE',  ( 0.000000000000000000, 0.000000000000000000, 1.000000000000000000 ) ) ;
#12265 = CARTESIAN_POINT ( 'NONE',  ( 2.694222958124177204E-15, 122.0000000000000000, 22.00000000000000355 ) ) ;
#12266 = ORIENTED_EDGE ( 'NONE', *, *, #11797, .T. ) ;
#12267 = DIRECTION ( 'NONE',  ( 0.000000000000000000, -0.000000000000000000, 1.000000000000000000 ) ) ;
#12268 = VECTOR ( 'NONE', #10976, 1000.000000000000000 ) ;
#12269 = EDGE_CURVE ( 'NONE', #2354, #1231, #11082, .T. ) ;
#12270 = FACE_OUTER_BOUND ( 'NONE', #12163, .T. ) ;
#12271 = VECTOR ( 'NONE', #7260, 1000.000000000000000 ) ;
#12272 = FILL_AREA_STYLE ('',( #8568 ) ) ;
#12273 = ORIENTED_EDGE ( 'NONE', *, *, #4742, .T. ) ;
#12274 = DIRECTION ( 'NONE',  ( 1.000000000000000000, -0.000000000000000000, 0.000000000000000000 ) ) ;
#12275 = CARTESIAN_POINT ( 'NONE',  ( 1.990051048614449116E-16, 113.2500000000000000, 3.250000000000000444 ) ) ;
#12276 = CARTESIAN_POINT ( 'NONE',  ( 70.80917463421377533, 19.14431278602349096, -24.94686153084484204 ) ) ;
#12277 = ORIENTED_EDGE ( 'NONE', *, *, #7107, .T. ) ;
#12278 = APPLICATION_CONTEXT ( 'automotive_design' ) ;
#12279 = DIRECTION ( 'NONE',  ( 0.000000000000000000, 1.000000000000000000, 0.000000000000000000 ) ) ;
#12280 = LINE ( 'NONE', #3488, #2580 ) ;
#12281 = VERTEX_POINT ( 'NONE', #3657 ) ;
#12282 = DIRECTION ( 'NONE',  ( 0.000000000000000000, 1.000000000000000000, 0.000000000000000000 ) ) ;
#12283 = AXIS2_PLACEMENT_3D ( 'NONE', #8500, #5467, #12264 ) ;
#12284 = ORIENTED_EDGE ( 'NONE', *, *, #6662, .F. ) ;
#12285 = ORIENTED_EDGE ( 'NONE', *, *, #7166, .T. ) ;
#12286 = LINE ( 'NONE', #8583, #11115 ) ;
#12287 = CARTESIAN_POINT ( 'NONE',  ( 25.00000000000000000, 347.0000000000000568, -88.00000000000000000 ) ) ;
#12288 = VERTEX_POINT ( 'NONE', #4532 ) ;
#12289 = CIRCLE ( 'NONE', #5524, 125.0000000000000284 ) ;
#12290 = DIRECTION ( 'NONE',  ( -0.000000000000000000, -1.000000000000000000, -0.000000000000000000 ) ) ;
#12291 = ORIENTED_EDGE ( 'NONE', *, *, #10228, .F. ) ;
#12292 = CARTESIAN_POINT ( 'NONE',  ( 0.000000000000000000, 0.000000000000000000, 0.000000000000000000 ) ) ;
#12293 = CARTESIAN_POINT ( 'NONE',  ( 0.000000000000000000, 216.0365690573663926, -10.49999999999999822 ) ) ;
#12294 = B_SPLINE_CURVE_WITH_KNOTS ( 'NONE', 3,
 ( #3198, #7867, #2080, #264 ),
 .UNSPECIFIED., .F., .F.,
 ( 4, 4 ),
 ( 0.0002502309401075617249, 0.0005002309401076790408 ),
 .UNSPECIFIED. ) ;
#12295 = DIRECTION ( 'NONE',  ( 0.000000000000000000, 0.000000000000000000, 1.000000000000000000 ) ) ;
#12296 = DIRECTION ( 'NONE',  ( 0.000000000000000000, -0.000000000000000000, -1.000000000000000000 ) ) ;
#12297 = ORIENTED_EDGE ( 'NONE', *, *, #4955, .F. ) ;
#12298 = CARTESIAN_POINT ( 'NONE',  ( -1.121994411437818862, 111.8749999986343937, 2.708734124999999882 ) ) ;
#12299 = EDGE_CURVE ( 'NONE', #712, #5882, #7519, .T. ) ;
#12300 = DIRECTION ( 'NONE',  ( 0.000000000000000000, 0.000000000000000000, 1.000000000000000000 ) ) ;
#12301 = ORIENTED_EDGE ( 'NONE', *, *, #6788, .T. ) ;
#12302 = LINE ( 'NONE', #2132, #3771 ) ;
#12303 = CARTESIAN_POINT ( 'NONE',  ( 72.45461974811382788, 50.00000000000007105, 19.38446435976420190 ) ) ;
#12304 = ORIENTED_EDGE ( 'NONE', *, *, #5007, .T. ) ;
#12305 = CARTESIAN_POINT ( 'NONE',  ( 1.346194077712557391, 110.1875000000000000, 3.250000000000002220 ) ) ;
#12306 = CARTESIAN_POINT ( 'NONE',  ( 72.46134176498804891, 49.99999999923035432, 19.35843010035742040 ) ) ;
#12307 = VERTEX_POINT ( 'NONE', #2600 ) ;
#12308 = CARTESIAN_POINT ( 'NONE',  ( 21.00000000000000355, 0.000000000000000000, 2.055000000000000160 ) ) ;
#12309 = DIRECTION ( 'NONE',  ( -0.5000000000000016653, -0.8660254037844378194, 0.000000000000000000 ) ) ;
#12310 = CARTESIAN_POINT ( 'NONE',  ( 2.298097038856278918, 114.7499999972688158, -2.298097038856279806 ) ) ;
#12311 = DIRECTION ( 'NONE',  ( -0.000000000000000000, -0.000000000000000000, 1.000000000000000000 ) ) ;
#12312 = ORIENTED_EDGE ( 'NONE', *, *, #3308, .F. ) ;
#12313 = VECTOR ( 'NONE', #498, 1000.000000000000000 ) ;
#12314 =( BOUNDED_CURVE ( )  B_SPLINE_CURVE ( 2, ( #2109, #8575, #101, #7653, #10580, #5669, #7773, #11591, #7833 ),
 .UNSPECIFIED., .F., .F. ) 
 B_SPLINE_CURVE_WITH_KNOTS ( ( 3, 2, 2, 2, 3 ),
 ( 0.3125000000000002776, 0.3437500000000003331, 0.3750000000000003331, 0.4062500000000003331, 0.4375000000000003886 ),
 .UNSPECIFIED. ) 
 CURVE ( )  GEOMETRIC_REPRESENTATION_ITEM ( )  RATIONAL_B_SPLINE_CURVE ( ( 0.9999999999999993339, 0.9238795325112874046, 1.000000000000000000, 0.9238795325112867385, 1.000000000000000000, 0.9238795325112867385, 1.000000000000000000, 0.9238795325112857393, 1.000000000000000888 ) ) 
 REPRESENTATION_ITEM ( '' )  );
#12315 = ORIENTED_EDGE ( 'NONE', *, *, #5382, .F. ) ;
#12316 =( NAMED_UNIT ( * ) SI_UNIT ( $, .STERADIAN. ) SOLID_ANGLE_UNIT ( ) );
#12317 = LINE ( 'NONE', #4643, #8519 ) ;
#12318 = ORIENTED_EDGE ( 'NONE', *, *, #11515, .T. ) ;
#12319 = PLANE ( 'NONE',  #6424 ) ;
#12320 = DIRECTION ( 'NONE',  ( 0.000000000000000000, 0.000000000000000000, 1.000000000000000000 ) ) ;
#12321 = CARTESIAN_POINT ( 'NONE',  ( -20.00000000000000355, 63.00000000000000000, -57.08203932499370836 ) ) ;
#12322 = CIRCLE ( 'NONE', #11723, 28.00000000000000355 ) ;
#12323 = PLANE ( 'NONE',  #8188 ) ;
#12324 = PLANE ( 'NONE',  #11051 ) ;
#12325 = ORIENTED_EDGE ( 'NONE', *, *, #3293, .F. ) ;
#12326 = ADVANCED_FACE ( 'NONE', ( #11331 ), #739, .T. ) ;
#12327 = SURFACE_SIDE_STYLE ('',( #2969 ) ) ;
#12328 = ADVANCED_FACE ( 'NONE', ( #6586 ), #2718, .F. ) ;
#12329 = EDGE_CURVE ( 'NONE', #2134, #4117, #6971, .T. ) ;
#12330 = CARTESIAN_POINT ( 'NONE',  ( 70.79098555865897424, 40.21264271670013102, -24.99999999997160316 ) ) ;
#12331 = FACE_OUTER_BOUND ( 'NONE', #8036, .T. ) ;
#12332 = ORIENTED_EDGE ( 'NONE', *, *, #4193, .T. ) ;
#12333 = CARTESIAN_POINT ( 'NONE',  ( 28.20745110743105499, 86.12135132227002998, 11.13838988601293778 ) ) ;
#12334 = LINE ( 'NONE', #3723, #707 ) ;
#12335 = CARTESIAN_POINT ( 'NONE',  ( 165.0000000000011369, 0.000000000000000000, 25.00000000000000000 ) ) ;
#12336 = ORIENTED_EDGE ( 'NONE', *, *, #10028, .T. ) ;
#12337 = DIRECTION ( 'NONE',  ( 0.4999999999999914513, -0.8660254037844435926, 0.000000000000000000 ) ) ;
#12338 = LINE ( 'NONE', #4853, #384 ) ;
#12339 = CIRCLE ( 'NONE', #4167, 5.000000000000000888 ) ;
#12340 = CIRCLE ( 'NONE', #3174, 9.999999999999994671 ) ;
#12341 = VERTEX_POINT ( 'NONE', #2541 ) ;
#12342 = CARTESIAN_POINT ( 'NONE',  ( 5.525725221640833240, 18.86666975080242992, 80.00000000000000000 ) ) ;
#12343 = EDGE_CURVE ( 'NONE', #12042, #7445, #10129, .T. ) ;
#12344 = ADVANCED_FACE ( 'NONE', ( #12146 ), #670, .F. ) ;
#12345 = VERTEX_POINT ( 'NONE', #5537 ) ;
#12346 = DIRECTION ( 'NONE',  ( -0.8660254037844394848, -0.4999999999999985012, 0.000000000000000000 ) ) ;
#12347 = CIRCLE ( 'NONE', #8753, 12.99999999999999822 ) ;
#12348 = CARTESIAN_POINT ( 'NONE',  ( 20.00000000000000355, 50.00000000000000000, 57.08203932499370836 ) ) ;
#12349 = ORIENTED_EDGE ( 'NONE', *, *, #9179, .F. ) ;
#12350 = DIRECTION ( 'NONE',  ( 0.000000000000000000, 1.000000000000000000, 0.000000000000000000 ) ) ;
#12351 = VERTEX_POINT ( 'NONE', #9748 ) ;
#12352 = PRODUCT_CONTEXT ( 'NONE', #8674, 'mechanical' ) ;
#12353 = CARTESIAN_POINT ( 'NONE',  ( -45.35898384862240107, 67.00000000000008527, 25.98076211353315657 ) ) ;
#12354 = NEXT_ASSEMBLY_USAGE_OCCURRENCE ( 'NAUO1', ' ', ' ', #4743, #11834, $ ) ;
#12355 = NEXT_ASSEMBLY_USAGE_OCCURRENCE ( 'NAUO2', ' ', ' ', #4743, #5048, $ ) ;
#12356 = NEXT_ASSEMBLY_USAGE_OCCURRENCE ( 'NAUO3', ' ', ' ', #4743, #5201, $ ) ;
#12357 = NEXT_ASSEMBLY_USAGE_OCCURRENCE ( 'NAUO4', ' ', ' ', #4743, #7780, $ ) ;
#12358 = NEXT_ASSEMBLY_USAGE_OCCURRENCE ( 'NAUO5', ' ', ' ', #4743, #545, $ ) ;
#12359 = NEXT_ASSEMBLY_USAGE_OCCURRENCE ( 'NAUO6', ' ', ' ', #4743, #869, $ ) ;
#12360 = NEXT_ASSEMBLY_USAGE_OCCURRENCE ( 'NAUO7', ' ', ' ', #4743, #3674, $ ) ;
#12361 = NEXT_ASSEMBLY_USAGE_OCCURRENCE ( 'NAUO8', ' ', ' ', #4743, #11612, $ ) ;
ENDSEC;
END-ISO-10303-21;
